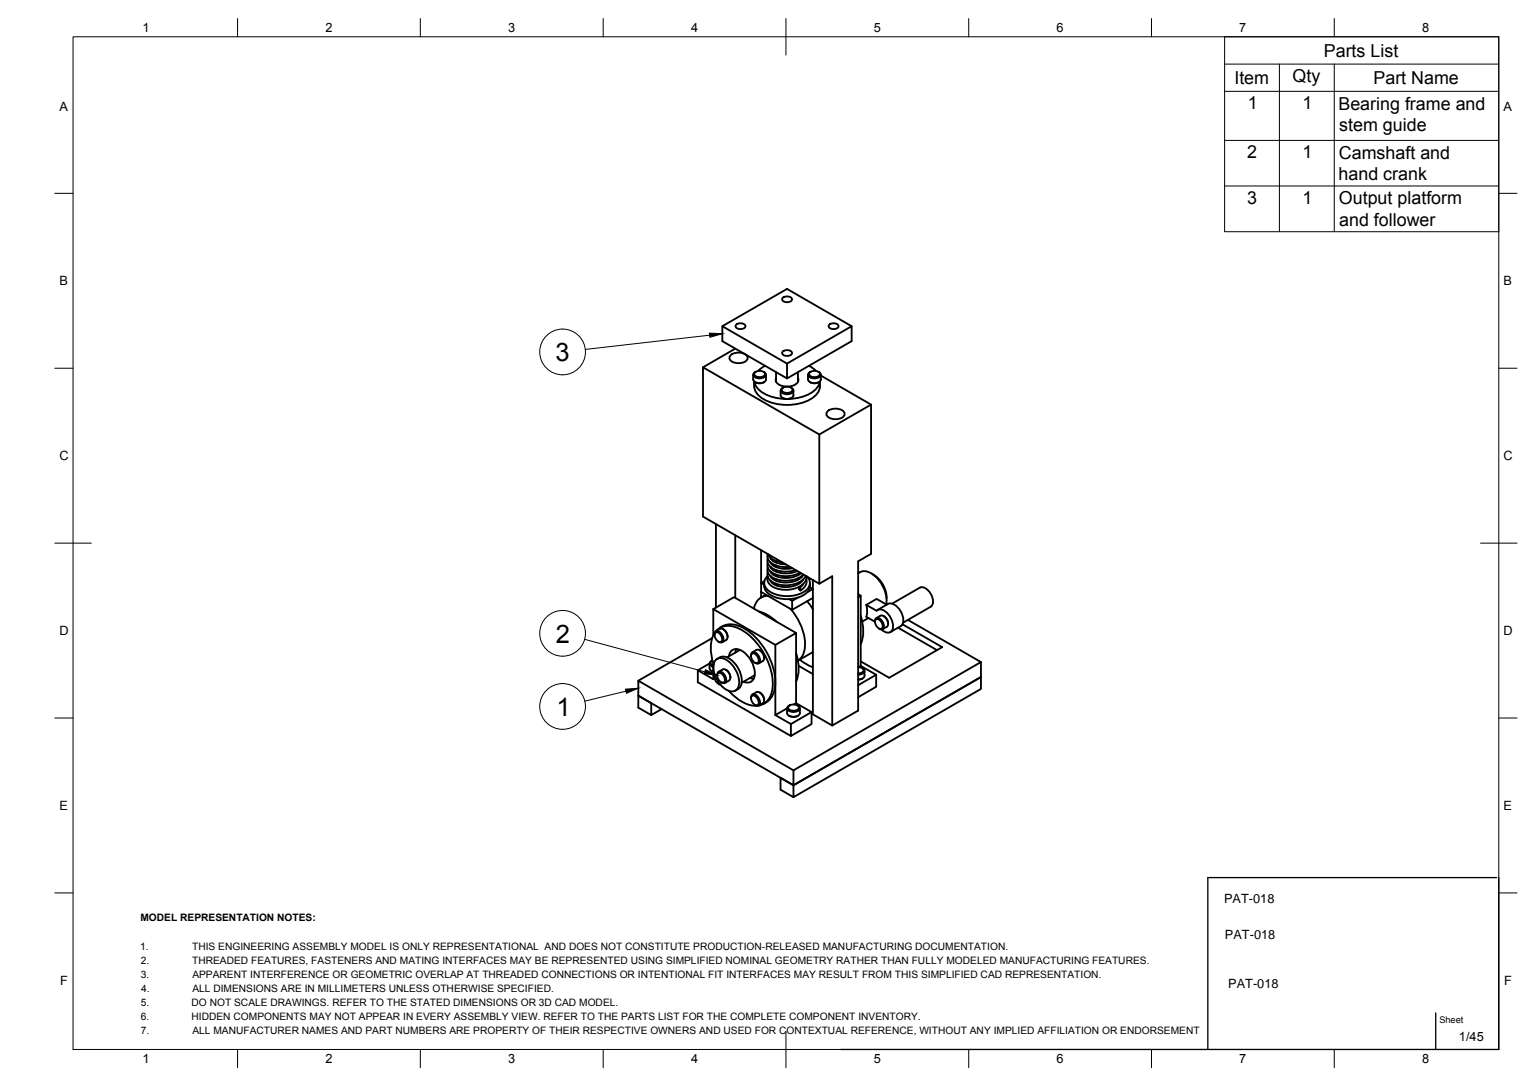
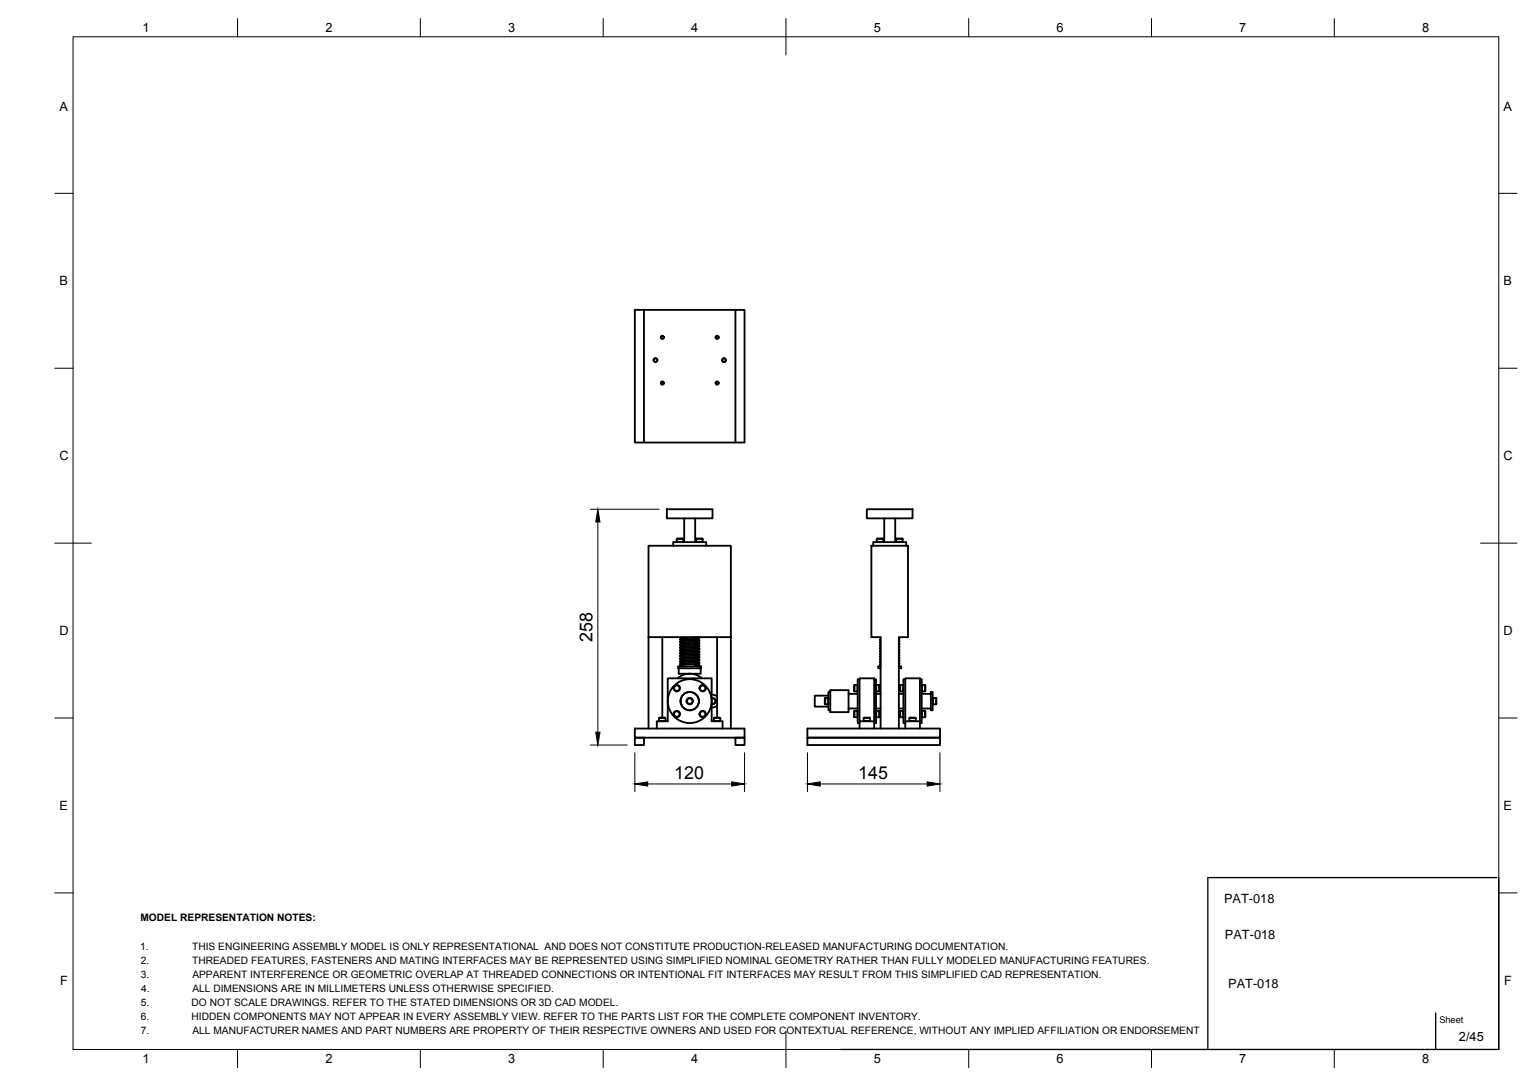
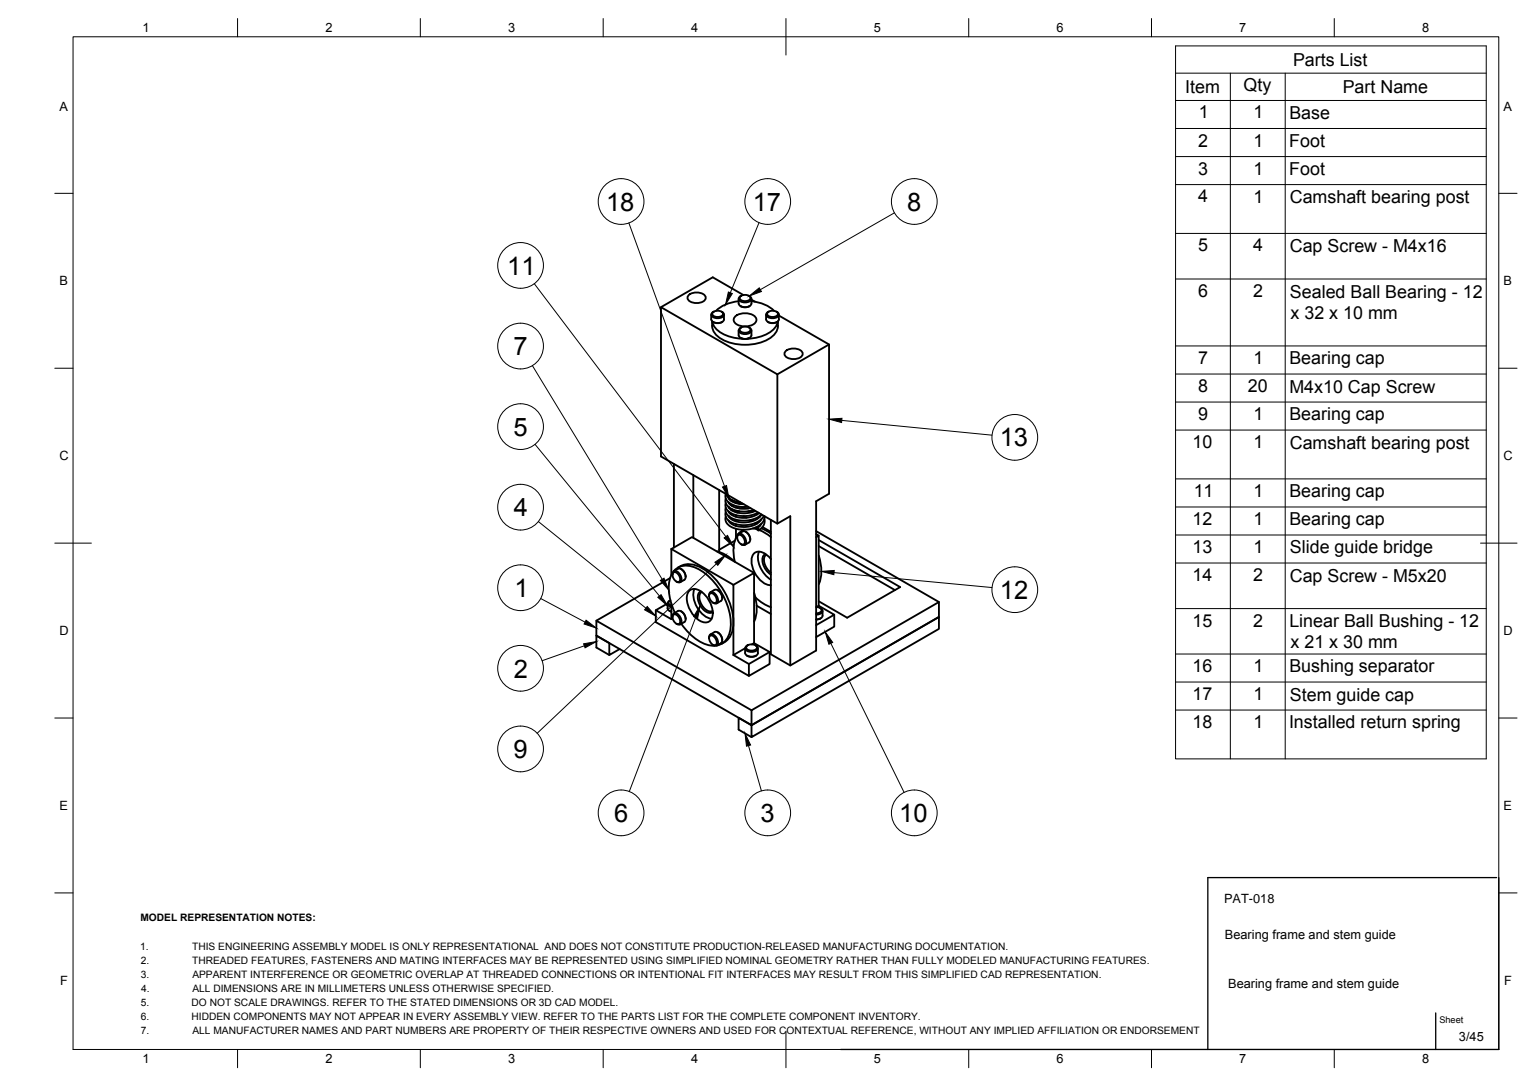
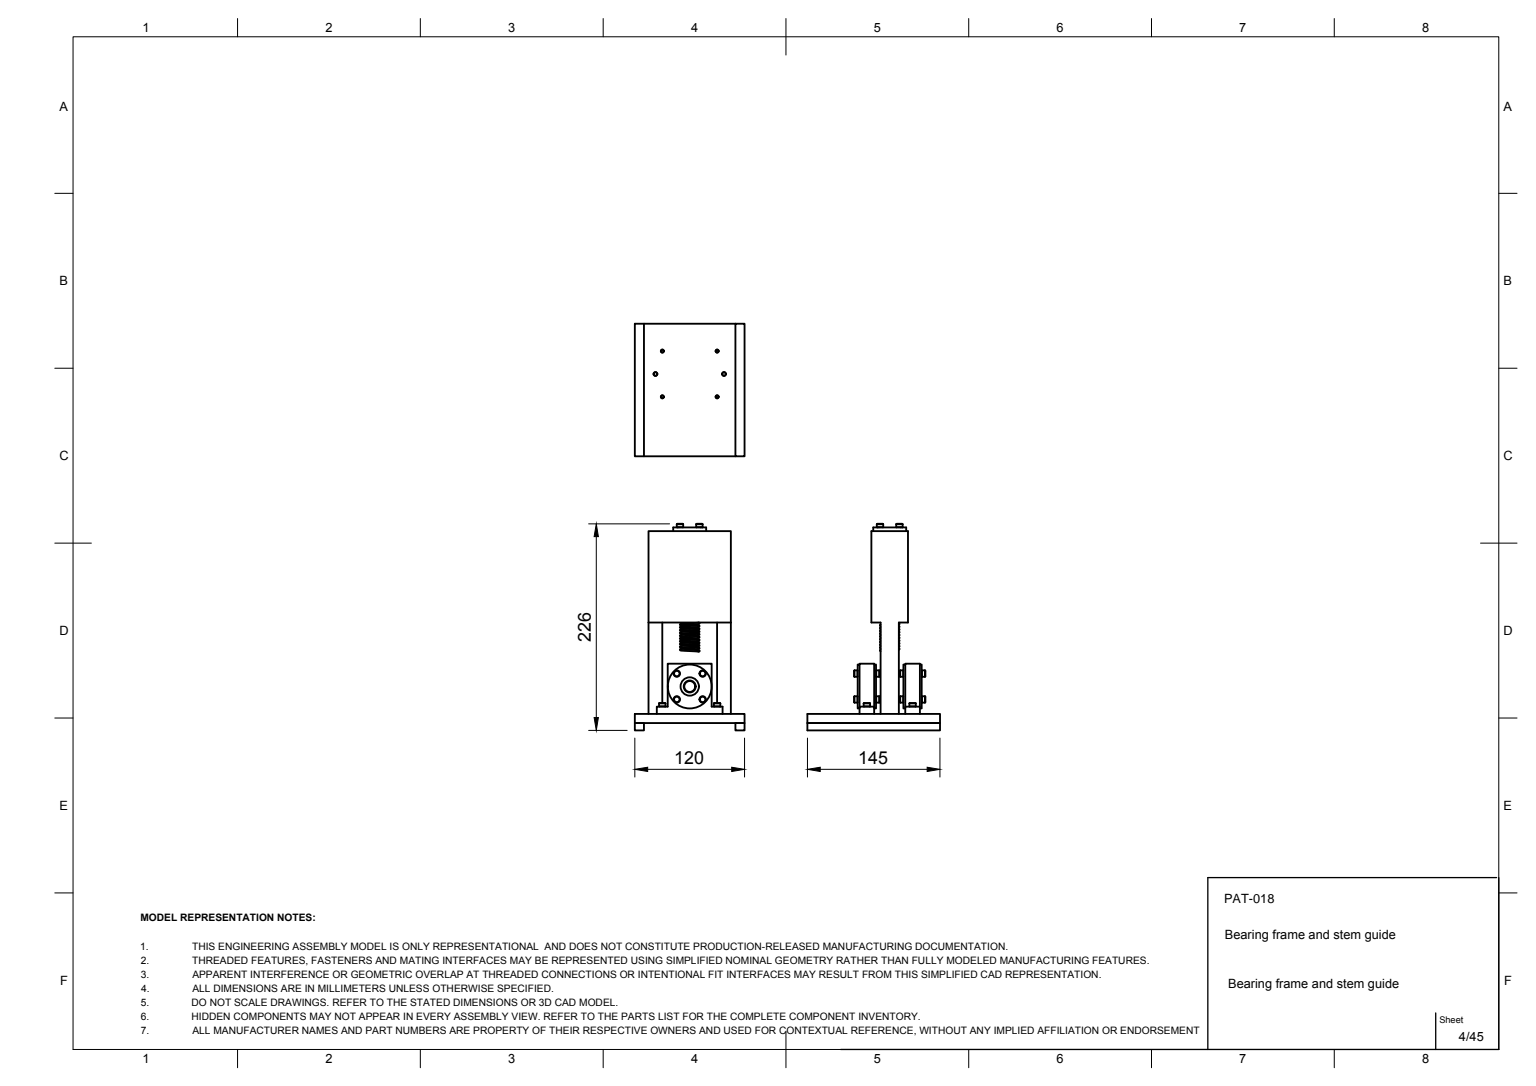
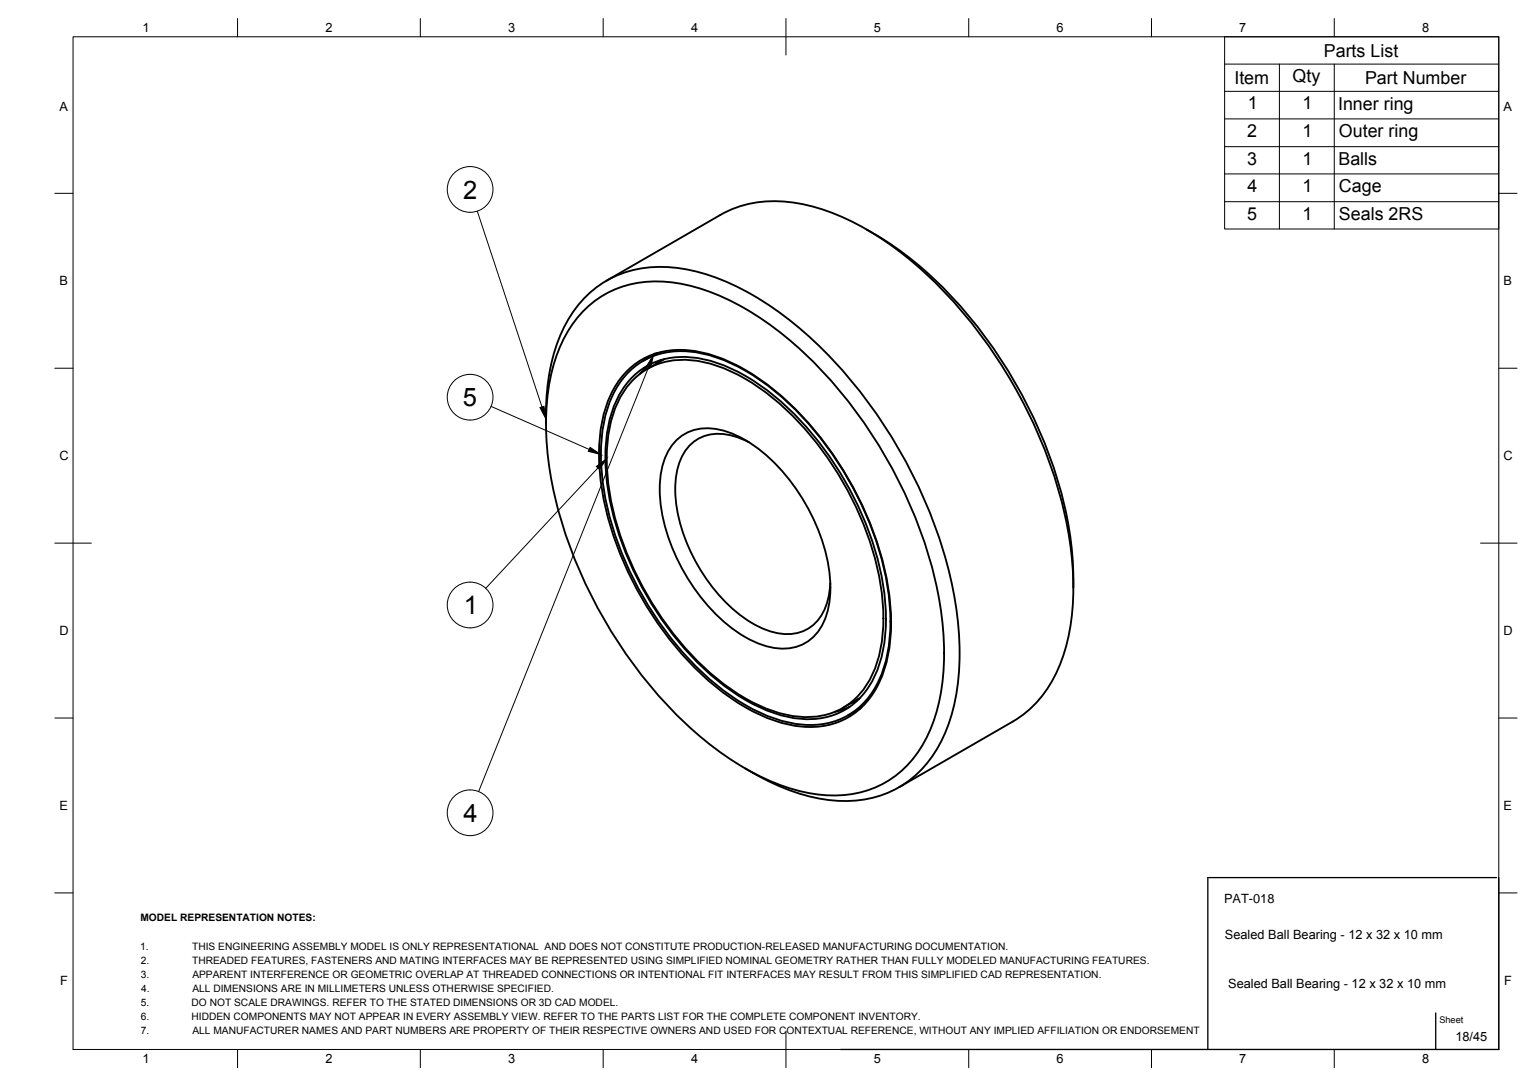
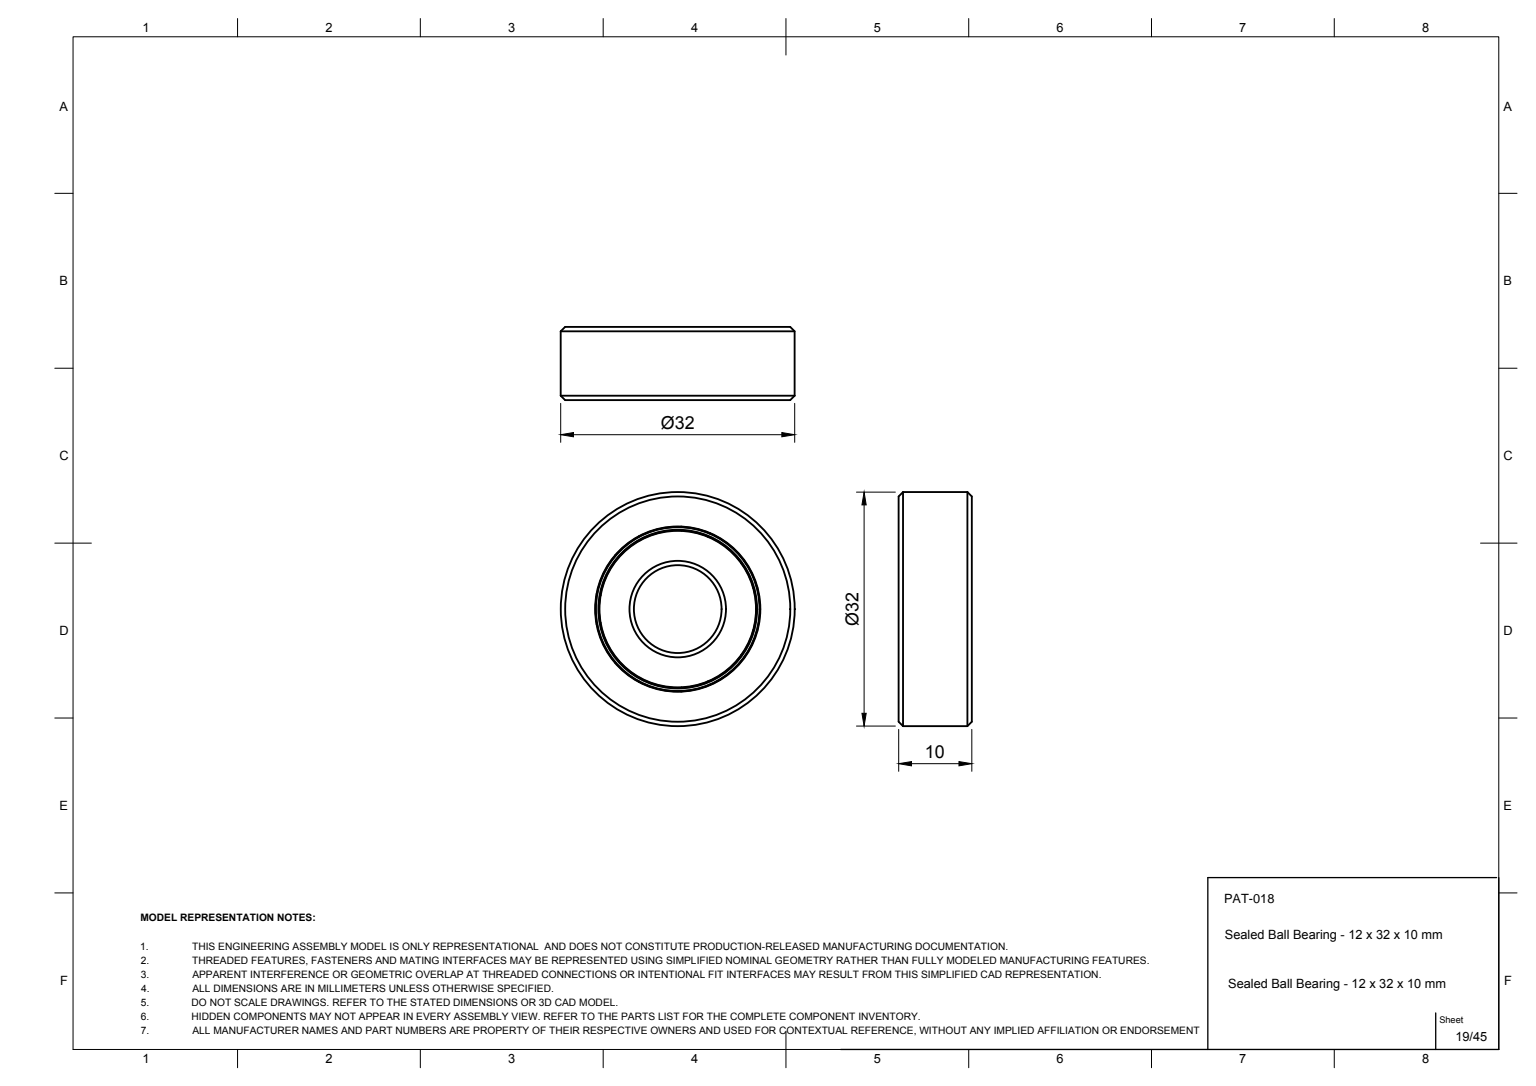
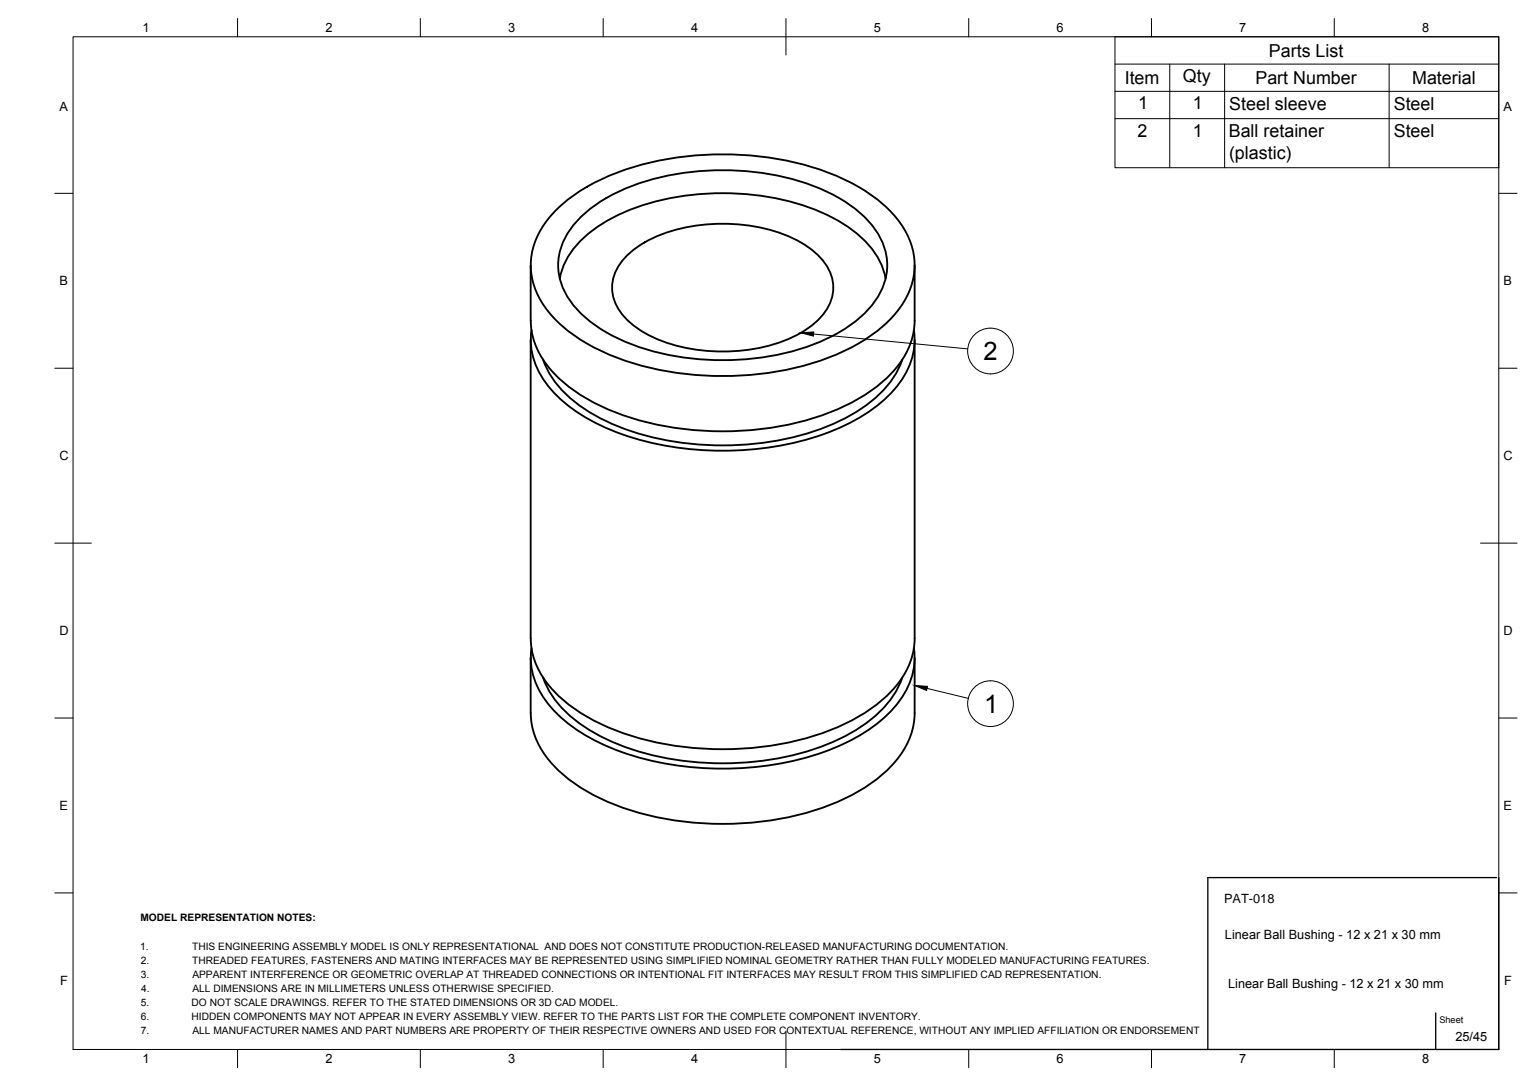
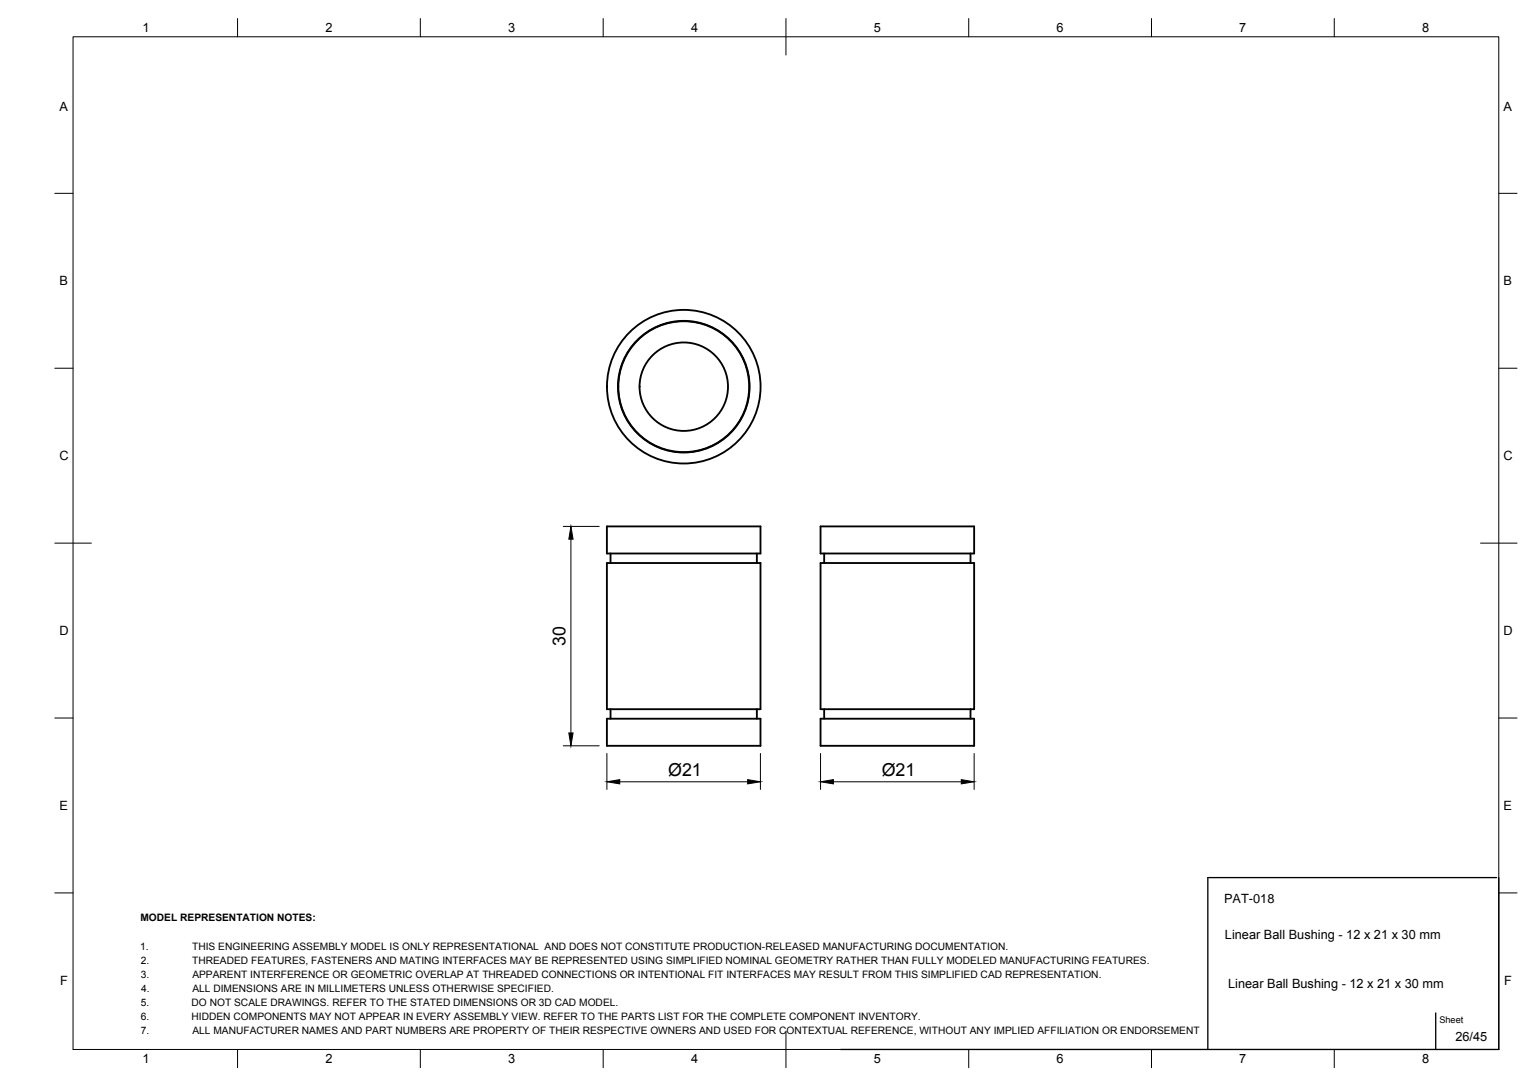
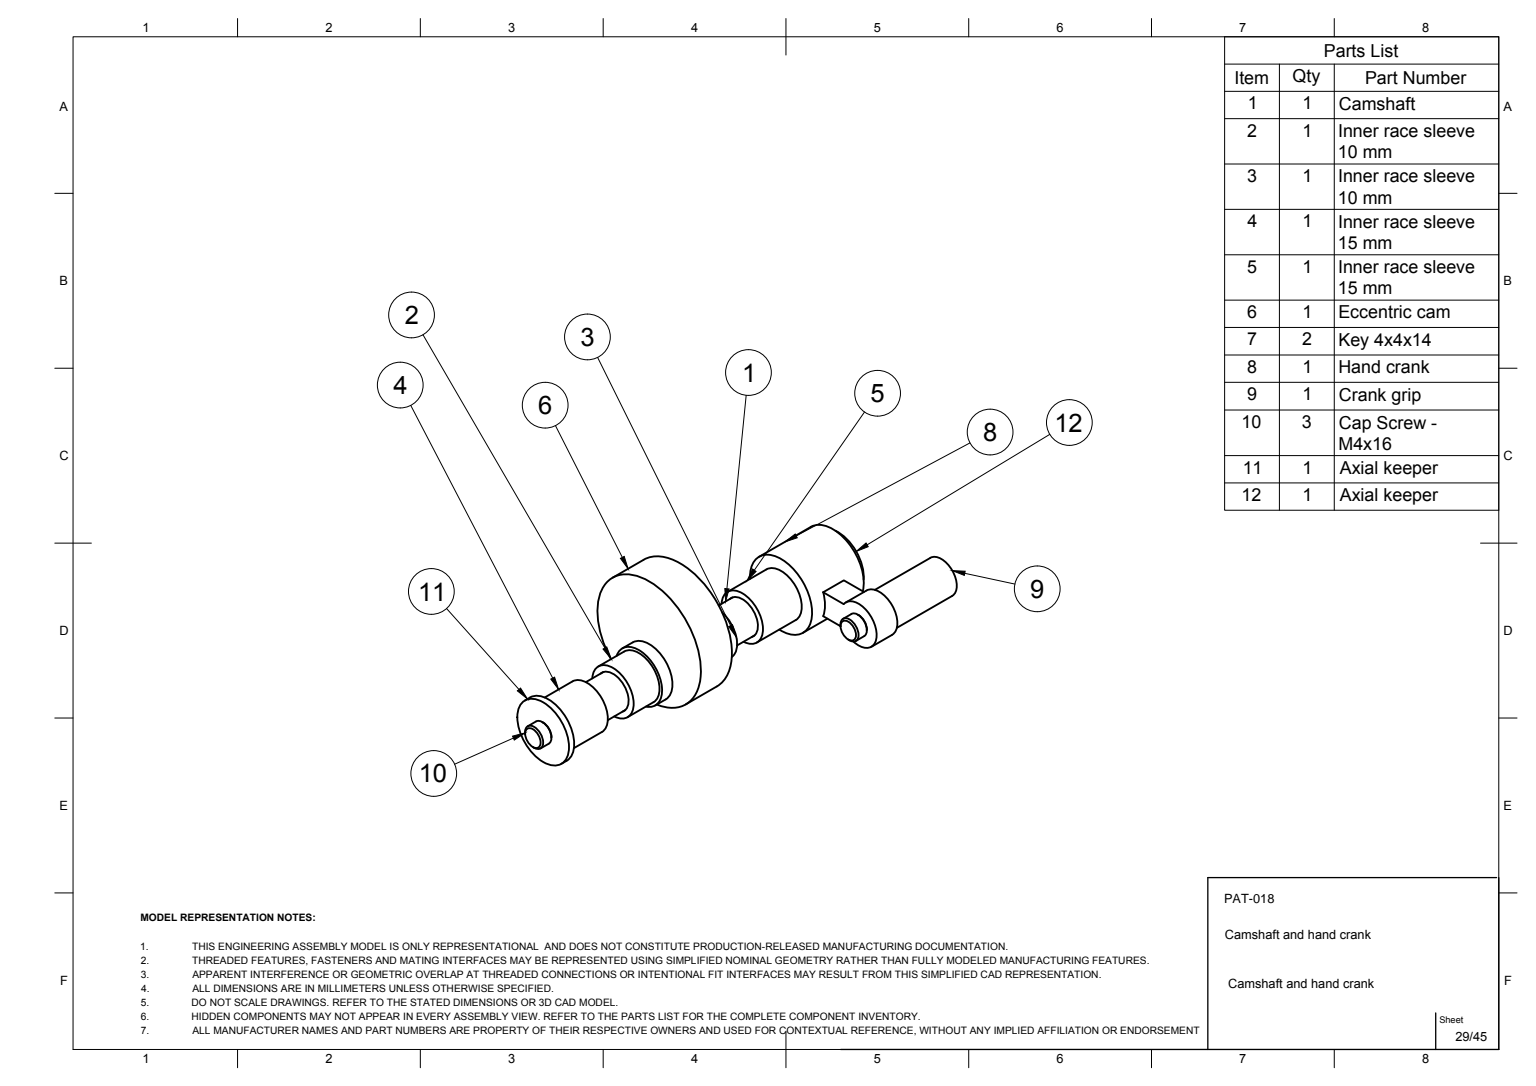
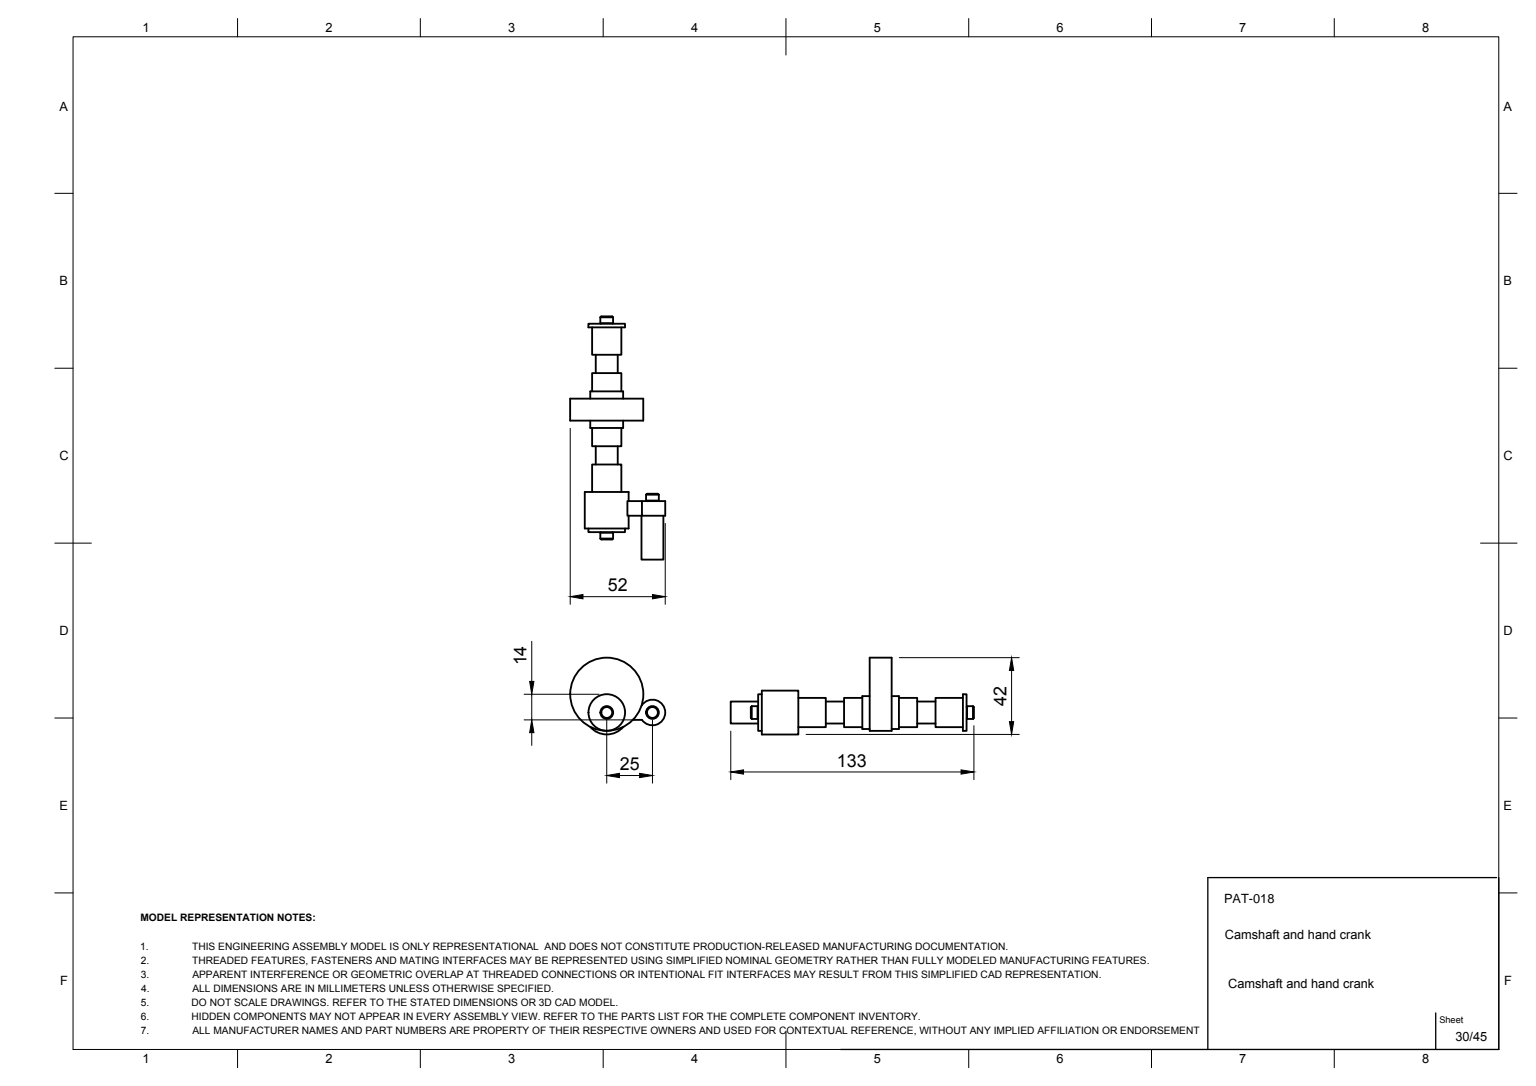
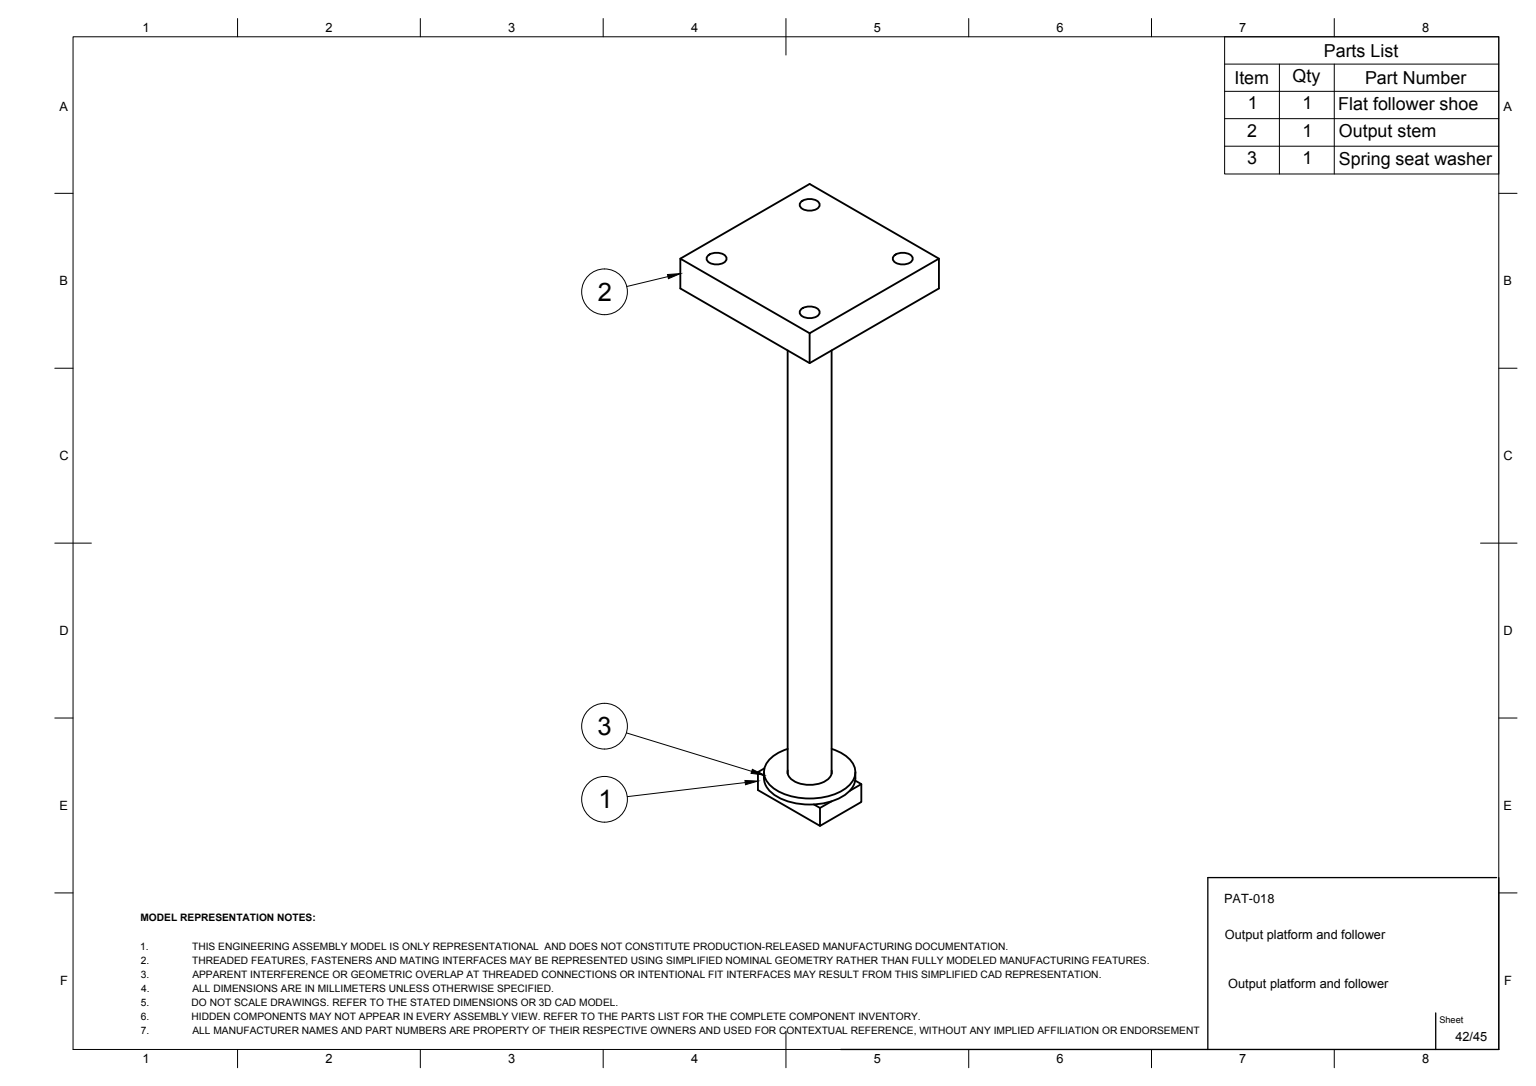
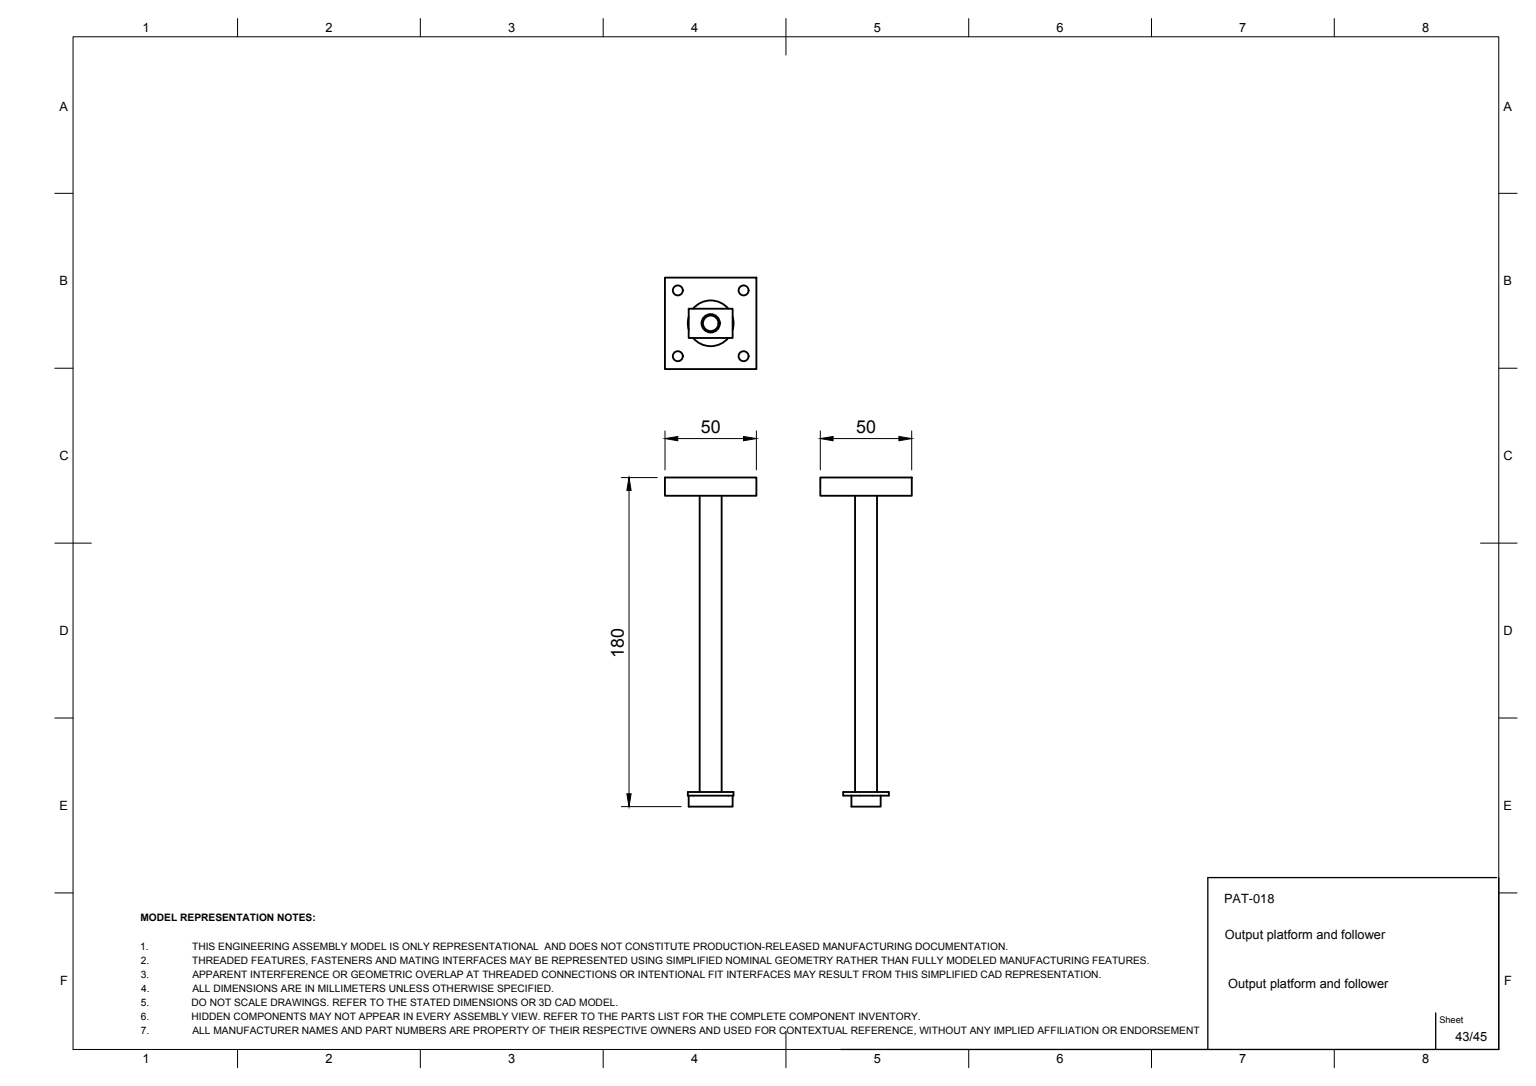
ISO-10303-21;
HEADER;
/* Generated by software containing ST-Developer
 * from STEP Tools, Inc. (www.steptools.com) 
 */

FILE_DESCRIPTION(
/* description */ ('Cam-driven reciprocating slide'),
/* implementation_level */ '2;1');

FILE_NAME(
/* name */ 'PAT-018',
/* time_stamp */ '2026-10-28T03:25:20-07:00',
/* author */ (''),
/* organization */ (''),
/* preprocessor_version */ 'ST-DEVELOPER v20.2',
/* originating_system */ 'Autodesk Translation Framework v15.17.0.0',
/* authorisation */ '');

FILE_SCHEMA (('AUTOMOTIVE_DESIGN { 1 0 10303 214 3 1 1 }'));
ENDSEC;

DATA;
#10=MECHANICAL_DESIGN_GEOMETRIC_PRESENTATION_REPRESENTATION('',(#422,#423,
#424,#425,#426,#427,#428,#429,#430,#431,#432,#433,#434,#435,#436,#437,#438,
#439,#440,#441,#442,#443,#444,#445,#446,#447,#448,#449,#450,#451,#452,#453,
#454,#455,#456,#457,#458,#459,#460,#461,#462,#463,#464,#465),#13277);
#11=ORIENTED_CLOSED_SHELL('',*,#6424,.F.);
#12=ORIENTED_CLOSED_SHELL('',*,#6427,.F.);
#13=ORIENTED_CLOSED_SHELL('',*,#6441,.F.);
#14=BREP_WITH_VOIDS('Body1',#6423,(#11));
#15=BREP_WITH_VOIDS('Body1',#6428,(#12));
#16=BREP_WITH_VOIDS('Body1',#6440,(#13));
#17=ITEM_DEFINED_TRANSFORMATION($,$,#7155,#7277);
#18=ITEM_DEFINED_TRANSFORMATION($,$,#7175,#7278);
#19=ITEM_DEFINED_TRANSFORMATION($,$,#7195,#7279);
#20=ITEM_DEFINED_TRANSFORMATION($,$,#7210,#7280);
#21=ITEM_DEFINED_TRANSFORMATION($,$,#7260,#7281);
#22=ITEM_DEFINED_TRANSFORMATION($,$,#7309,#7358);
#23=ITEM_DEFINED_TRANSFORMATION($,$,#7341,#7359);
#24=ITEM_DEFINED_TRANSFORMATION($,$,#6855,#7558);
#25=ITEM_DEFINED_TRANSFORMATION($,$,#6885,#7559);
#26=ITEM_DEFINED_TRANSFORMATION($,$,#6892,#7560);
#27=ITEM_DEFINED_TRANSFORMATION($,$,#6899,#7561);
#28=ITEM_DEFINED_TRANSFORMATION($,$,#6931,#7562);
#29=ITEM_DEFINED_TRANSFORMATION($,$,#6956,#7563);
#30=ITEM_DEFINED_TRANSFORMATION($,$,#6981,#7564);
#31=ITEM_DEFINED_TRANSFORMATION($,$,#7013,#7565);
#32=ITEM_DEFINED_TRANSFORMATION($,$,#7038,#7566);
#33=ITEM_DEFINED_TRANSFORMATION($,$,#7063,#7567);
#34=ITEM_DEFINED_TRANSFORMATION($,$,#7115,#7568);
#35=ITEM_DEFINED_TRANSFORMATION($,$,#7124,#7569);
#36=ITEM_DEFINED_TRANSFORMATION($,$,#7149,#7570);
#37=ITEM_DEFINED_TRANSFORMATION($,$,#7532,#7571);
#38=ITEM_DEFINED_TRANSFORMATION($,$,#7532,#7572);
#39=ITEM_DEFINED_TRANSFORMATION($,$,#7154,#7573);
#40=ITEM_DEFINED_TRANSFORMATION($,$,#7360,#7574);
#41=ITEM_DEFINED_TRANSFORMATION($,$,#7360,#7575);
#42=ITEM_DEFINED_TRANSFORMATION($,$,#7360,#7576);
#43=ITEM_DEFINED_TRANSFORMATION($,$,#7360,#7577);
#44=ITEM_DEFINED_TRANSFORMATION($,$,#7360,#7578);
#45=ITEM_DEFINED_TRANSFORMATION($,$,#7360,#7579);
#46=ITEM_DEFINED_TRANSFORMATION($,$,#7360,#7580);
#47=ITEM_DEFINED_TRANSFORMATION($,$,#7360,#7581);
#48=ITEM_DEFINED_TRANSFORMATION($,$,#7532,#7582);
#49=ITEM_DEFINED_TRANSFORMATION($,$,#7532,#7583);
#50=ITEM_DEFINED_TRANSFORMATION($,$,#7154,#7584);
#51=ITEM_DEFINED_TRANSFORMATION($,$,#7360,#7585);
#52=ITEM_DEFINED_TRANSFORMATION($,$,#7360,#7586);
#53=ITEM_DEFINED_TRANSFORMATION($,$,#7360,#7587);
#54=ITEM_DEFINED_TRANSFORMATION($,$,#7360,#7588);
#55=ITEM_DEFINED_TRANSFORMATION($,$,#7360,#7589);
#56=ITEM_DEFINED_TRANSFORMATION($,$,#7360,#7590);
#57=ITEM_DEFINED_TRANSFORMATION($,$,#7360,#7591);
#58=ITEM_DEFINED_TRANSFORMATION($,$,#7360,#7592);
#59=ITEM_DEFINED_TRANSFORMATION($,$,#7282,#7593);
#60=ITEM_DEFINED_TRANSFORMATION($,$,#7282,#7594);
#61=ITEM_DEFINED_TRANSFORMATION($,$,#7308,#7595);
#62=ITEM_DEFINED_TRANSFORMATION($,$,#7308,#7596);
#63=ITEM_DEFINED_TRANSFORMATION($,$,#7360,#7597);
#64=ITEM_DEFINED_TRANSFORMATION($,$,#7360,#7598);
#65=ITEM_DEFINED_TRANSFORMATION($,$,#7360,#7599);
#66=ITEM_DEFINED_TRANSFORMATION($,$,#7360,#7600);
#67=ITEM_DEFINED_TRANSFORMATION($,$,#7385,#7601);
#68=ITEM_DEFINED_TRANSFORMATION($,$,#7413,#7602);
#69=ITEM_DEFINED_TRANSFORMATION($,$,#7422,#7603);
#70=ITEM_DEFINED_TRANSFORMATION($,$,#7431,#7604);
#71=ITEM_DEFINED_TRANSFORMATION($,$,#7440,#7605);
#72=ITEM_DEFINED_TRANSFORMATION($,$,#7449,#7606);
#73=ITEM_DEFINED_TRANSFORMATION($,$,#7469,#7607);
#74=ITEM_DEFINED_TRANSFORMATION($,$,#7493,#7608);
#75=ITEM_DEFINED_TRANSFORMATION($,$,#7503,#7609);
#76=ITEM_DEFINED_TRANSFORMATION($,$,#7512,#7610);
#77=ITEM_DEFINED_TRANSFORMATION($,$,#7521,#7611);
#78=ITEM_DEFINED_TRANSFORMATION($,$,#7521,#7612);
#79=ITEM_DEFINED_TRANSFORMATION($,$,#7532,#7613);
#80=ITEM_DEFINED_TRANSFORMATION($,$,#7532,#7614);
#81=ITEM_DEFINED_TRANSFORMATION($,$,#7532,#7615);
#82=ITEM_DEFINED_TRANSFORMATION($,$,#7617,#7663);
#83=ITEM_DEFINED_TRANSFORMATION($,$,#7627,#7664);
#84=ITEM_DEFINED_TRANSFORMATION($,$,#7654,#7665);
#85=ITEM_DEFINED_TRANSFORMATION($,$,#6854,#7666);
#86=ITEM_DEFINED_TRANSFORMATION($,$,#7384,#7667);
#87=ITEM_DEFINED_TRANSFORMATION($,$,#7616,#7668);
#88=(
REPRESENTATION_RELATIONSHIP($,$,#13455,#13454)
REPRESENTATION_RELATIONSHIP_WITH_TRANSFORMATION(#17)
SHAPE_REPRESENTATION_RELATIONSHIP()
);
#89=(
REPRESENTATION_RELATIONSHIP($,$,#13456,#13454)
REPRESENTATION_RELATIONSHIP_WITH_TRANSFORMATION(#18)
SHAPE_REPRESENTATION_RELATIONSHIP()
);
#90=(
REPRESENTATION_RELATIONSHIP($,$,#13457,#13454)
REPRESENTATION_RELATIONSHIP_WITH_TRANSFORMATION(#19)
SHAPE_REPRESENTATION_RELATIONSHIP()
);
#91=(
REPRESENTATION_RELATIONSHIP($,$,#13458,#13454)
REPRESENTATION_RELATIONSHIP_WITH_TRANSFORMATION(#20)
SHAPE_REPRESENTATION_RELATIONSHIP()
);
#92=(
REPRESENTATION_RELATIONSHIP($,$,#13459,#13454)
REPRESENTATION_RELATIONSHIP_WITH_TRANSFORMATION(#21)
SHAPE_REPRESENTATION_RELATIONSHIP()
);
#93=(
REPRESENTATION_RELATIONSHIP($,$,#13462,#13461)
REPRESENTATION_RELATIONSHIP_WITH_TRANSFORMATION(#22)
SHAPE_REPRESENTATION_RELATIONSHIP()
);
#94=(
REPRESENTATION_RELATIONSHIP($,$,#13463,#13461)
REPRESENTATION_RELATIONSHIP_WITH_TRANSFORMATION(#23)
SHAPE_REPRESENTATION_RELATIONSHIP()
);
#95=(
REPRESENTATION_RELATIONSHIP($,$,#13441,#13440)
REPRESENTATION_RELATIONSHIP_WITH_TRANSFORMATION(#24)
SHAPE_REPRESENTATION_RELATIONSHIP()
);
#96=(
REPRESENTATION_RELATIONSHIP($,$,#13442,#13440)
REPRESENTATION_RELATIONSHIP_WITH_TRANSFORMATION(#25)
SHAPE_REPRESENTATION_RELATIONSHIP()
);
#97=(
REPRESENTATION_RELATIONSHIP($,$,#13443,#13440)
REPRESENTATION_RELATIONSHIP_WITH_TRANSFORMATION(#26)
SHAPE_REPRESENTATION_RELATIONSHIP()
);
#98=(
REPRESENTATION_RELATIONSHIP($,$,#13444,#13440)
REPRESENTATION_RELATIONSHIP_WITH_TRANSFORMATION(#27)
SHAPE_REPRESENTATION_RELATIONSHIP()
);
#99=(
REPRESENTATION_RELATIONSHIP($,$,#13445,#13440)
REPRESENTATION_RELATIONSHIP_WITH_TRANSFORMATION(#28)
SHAPE_REPRESENTATION_RELATIONSHIP()
);
#100=(
REPRESENTATION_RELATIONSHIP($,$,#13446,#13440)
REPRESENTATION_RELATIONSHIP_WITH_TRANSFORMATION(#29)
SHAPE_REPRESENTATION_RELATIONSHIP()
);
#101=(
REPRESENTATION_RELATIONSHIP($,$,#13447,#13440)
REPRESENTATION_RELATIONSHIP_WITH_TRANSFORMATION(#30)
SHAPE_REPRESENTATION_RELATIONSHIP()
);
#102=(
REPRESENTATION_RELATIONSHIP($,$,#13448,#13440)
REPRESENTATION_RELATIONSHIP_WITH_TRANSFORMATION(#31)
SHAPE_REPRESENTATION_RELATIONSHIP()
);
#103=(
REPRESENTATION_RELATIONSHIP($,$,#13449,#13440)
REPRESENTATION_RELATIONSHIP_WITH_TRANSFORMATION(#32)
SHAPE_REPRESENTATION_RELATIONSHIP()
);
#104=(
REPRESENTATION_RELATIONSHIP($,$,#13450,#13440)
REPRESENTATION_RELATIONSHIP_WITH_TRANSFORMATION(#33)
SHAPE_REPRESENTATION_RELATIONSHIP()
);
#105=(
REPRESENTATION_RELATIONSHIP($,$,#13451,#13440)
REPRESENTATION_RELATIONSHIP_WITH_TRANSFORMATION(#34)
SHAPE_REPRESENTATION_RELATIONSHIP()
);
#106=(
REPRESENTATION_RELATIONSHIP($,$,#13452,#13440)
REPRESENTATION_RELATIONSHIP_WITH_TRANSFORMATION(#35)
SHAPE_REPRESENTATION_RELATIONSHIP()
);
#107=(
REPRESENTATION_RELATIONSHIP($,$,#13453,#13440)
REPRESENTATION_RELATIONSHIP_WITH_TRANSFORMATION(#36)
SHAPE_REPRESENTATION_RELATIONSHIP()
);
#108=(
REPRESENTATION_RELATIONSHIP($,$,#13477,#13440)
REPRESENTATION_RELATIONSHIP_WITH_TRANSFORMATION(#37)
SHAPE_REPRESENTATION_RELATIONSHIP()
);
#109=(
REPRESENTATION_RELATIONSHIP($,$,#13477,#13440)
REPRESENTATION_RELATIONSHIP_WITH_TRANSFORMATION(#38)
SHAPE_REPRESENTATION_RELATIONSHIP()
);
#110=(
REPRESENTATION_RELATIONSHIP($,$,#13454,#13440)
REPRESENTATION_RELATIONSHIP_WITH_TRANSFORMATION(#39)
SHAPE_REPRESENTATION_RELATIONSHIP()
);
#111=(
REPRESENTATION_RELATIONSHIP($,$,#13464,#13440)
REPRESENTATION_RELATIONSHIP_WITH_TRANSFORMATION(#40)
SHAPE_REPRESENTATION_RELATIONSHIP()
);
#112=(
REPRESENTATION_RELATIONSHIP($,$,#13464,#13440)
REPRESENTATION_RELATIONSHIP_WITH_TRANSFORMATION(#41)
SHAPE_REPRESENTATION_RELATIONSHIP()
);
#113=(
REPRESENTATION_RELATIONSHIP($,$,#13464,#13440)
REPRESENTATION_RELATIONSHIP_WITH_TRANSFORMATION(#42)
SHAPE_REPRESENTATION_RELATIONSHIP()
);
#114=(
REPRESENTATION_RELATIONSHIP($,$,#13464,#13440)
REPRESENTATION_RELATIONSHIP_WITH_TRANSFORMATION(#43)
SHAPE_REPRESENTATION_RELATIONSHIP()
);
#115=(
REPRESENTATION_RELATIONSHIP($,$,#13464,#13440)
REPRESENTATION_RELATIONSHIP_WITH_TRANSFORMATION(#44)
SHAPE_REPRESENTATION_RELATIONSHIP()
);
#116=(
REPRESENTATION_RELATIONSHIP($,$,#13464,#13440)
REPRESENTATION_RELATIONSHIP_WITH_TRANSFORMATION(#45)
SHAPE_REPRESENTATION_RELATIONSHIP()
);
#117=(
REPRESENTATION_RELATIONSHIP($,$,#13464,#13440)
REPRESENTATION_RELATIONSHIP_WITH_TRANSFORMATION(#46)
SHAPE_REPRESENTATION_RELATIONSHIP()
);
#118=(
REPRESENTATION_RELATIONSHIP($,$,#13464,#13440)
REPRESENTATION_RELATIONSHIP_WITH_TRANSFORMATION(#47)
SHAPE_REPRESENTATION_RELATIONSHIP()
);
#119=(
REPRESENTATION_RELATIONSHIP($,$,#13477,#13440)
REPRESENTATION_RELATIONSHIP_WITH_TRANSFORMATION(#48)
SHAPE_REPRESENTATION_RELATIONSHIP()
);
#120=(
REPRESENTATION_RELATIONSHIP($,$,#13477,#13440)
REPRESENTATION_RELATIONSHIP_WITH_TRANSFORMATION(#49)
SHAPE_REPRESENTATION_RELATIONSHIP()
);
#121=(
REPRESENTATION_RELATIONSHIP($,$,#13454,#13440)
REPRESENTATION_RELATIONSHIP_WITH_TRANSFORMATION(#50)
SHAPE_REPRESENTATION_RELATIONSHIP()
);
#122=(
REPRESENTATION_RELATIONSHIP($,$,#13464,#13440)
REPRESENTATION_RELATIONSHIP_WITH_TRANSFORMATION(#51)
SHAPE_REPRESENTATION_RELATIONSHIP()
);
#123=(
REPRESENTATION_RELATIONSHIP($,$,#13464,#13440)
REPRESENTATION_RELATIONSHIP_WITH_TRANSFORMATION(#52)
SHAPE_REPRESENTATION_RELATIONSHIP()
);
#124=(
REPRESENTATION_RELATIONSHIP($,$,#13464,#13440)
REPRESENTATION_RELATIONSHIP_WITH_TRANSFORMATION(#53)
SHAPE_REPRESENTATION_RELATIONSHIP()
);
#125=(
REPRESENTATION_RELATIONSHIP($,$,#13464,#13440)
REPRESENTATION_RELATIONSHIP_WITH_TRANSFORMATION(#54)
SHAPE_REPRESENTATION_RELATIONSHIP()
);
#126=(
REPRESENTATION_RELATIONSHIP($,$,#13464,#13440)
REPRESENTATION_RELATIONSHIP_WITH_TRANSFORMATION(#55)
SHAPE_REPRESENTATION_RELATIONSHIP()
);
#127=(
REPRESENTATION_RELATIONSHIP($,$,#13464,#13440)
REPRESENTATION_RELATIONSHIP_WITH_TRANSFORMATION(#56)
SHAPE_REPRESENTATION_RELATIONSHIP()
);
#128=(
REPRESENTATION_RELATIONSHIP($,$,#13464,#13440)
REPRESENTATION_RELATIONSHIP_WITH_TRANSFORMATION(#57)
SHAPE_REPRESENTATION_RELATIONSHIP()
);
#129=(
REPRESENTATION_RELATIONSHIP($,$,#13464,#13440)
REPRESENTATION_RELATIONSHIP_WITH_TRANSFORMATION(#58)
SHAPE_REPRESENTATION_RELATIONSHIP()
);
#130=(
REPRESENTATION_RELATIONSHIP($,$,#13460,#13440)
REPRESENTATION_RELATIONSHIP_WITH_TRANSFORMATION(#59)
SHAPE_REPRESENTATION_RELATIONSHIP()
);
#131=(
REPRESENTATION_RELATIONSHIP($,$,#13460,#13440)
REPRESENTATION_RELATIONSHIP_WITH_TRANSFORMATION(#60)
SHAPE_REPRESENTATION_RELATIONSHIP()
);
#132=(
REPRESENTATION_RELATIONSHIP($,$,#13461,#13440)
REPRESENTATION_RELATIONSHIP_WITH_TRANSFORMATION(#61)
SHAPE_REPRESENTATION_RELATIONSHIP()
);
#133=(
REPRESENTATION_RELATIONSHIP($,$,#13461,#13440)
REPRESENTATION_RELATIONSHIP_WITH_TRANSFORMATION(#62)
SHAPE_REPRESENTATION_RELATIONSHIP()
);
#134=(
REPRESENTATION_RELATIONSHIP($,$,#13464,#13440)
REPRESENTATION_RELATIONSHIP_WITH_TRANSFORMATION(#63)
SHAPE_REPRESENTATION_RELATIONSHIP()
);
#135=(
REPRESENTATION_RELATIONSHIP($,$,#13464,#13440)
REPRESENTATION_RELATIONSHIP_WITH_TRANSFORMATION(#64)
SHAPE_REPRESENTATION_RELATIONSHIP()
);
#136=(
REPRESENTATION_RELATIONSHIP($,$,#13464,#13440)
REPRESENTATION_RELATIONSHIP_WITH_TRANSFORMATION(#65)
SHAPE_REPRESENTATION_RELATIONSHIP()
);
#137=(
REPRESENTATION_RELATIONSHIP($,$,#13464,#13440)
REPRESENTATION_RELATIONSHIP_WITH_TRANSFORMATION(#66)
SHAPE_REPRESENTATION_RELATIONSHIP()
);
#138=(
REPRESENTATION_RELATIONSHIP($,$,#13466,#13465)
REPRESENTATION_RELATIONSHIP_WITH_TRANSFORMATION(#67)
SHAPE_REPRESENTATION_RELATIONSHIP()
);
#139=(
REPRESENTATION_RELATIONSHIP($,$,#13467,#13465)
REPRESENTATION_RELATIONSHIP_WITH_TRANSFORMATION(#68)
SHAPE_REPRESENTATION_RELATIONSHIP()
);
#140=(
REPRESENTATION_RELATIONSHIP($,$,#13468,#13465)
REPRESENTATION_RELATIONSHIP_WITH_TRANSFORMATION(#69)
SHAPE_REPRESENTATION_RELATIONSHIP()
);
#141=(
REPRESENTATION_RELATIONSHIP($,$,#13469,#13465)
REPRESENTATION_RELATIONSHIP_WITH_TRANSFORMATION(#70)
SHAPE_REPRESENTATION_RELATIONSHIP()
);
#142=(
REPRESENTATION_RELATIONSHIP($,$,#13470,#13465)
REPRESENTATION_RELATIONSHIP_WITH_TRANSFORMATION(#71)
SHAPE_REPRESENTATION_RELATIONSHIP()
);
#143=(
REPRESENTATION_RELATIONSHIP($,$,#13471,#13465)
REPRESENTATION_RELATIONSHIP_WITH_TRANSFORMATION(#72)
SHAPE_REPRESENTATION_RELATIONSHIP()
);
#144=(
REPRESENTATION_RELATIONSHIP($,$,#13472,#13465)
REPRESENTATION_RELATIONSHIP_WITH_TRANSFORMATION(#73)
SHAPE_REPRESENTATION_RELATIONSHIP()
);
#145=(
REPRESENTATION_RELATIONSHIP($,$,#13473,#13465)
REPRESENTATION_RELATIONSHIP_WITH_TRANSFORMATION(#74)
SHAPE_REPRESENTATION_RELATIONSHIP()
);
#146=(
REPRESENTATION_RELATIONSHIP($,$,#13474,#13465)
REPRESENTATION_RELATIONSHIP_WITH_TRANSFORMATION(#75)
SHAPE_REPRESENTATION_RELATIONSHIP()
);
#147=(
REPRESENTATION_RELATIONSHIP($,$,#13475,#13465)
REPRESENTATION_RELATIONSHIP_WITH_TRANSFORMATION(#76)
SHAPE_REPRESENTATION_RELATIONSHIP()
);
#148=(
REPRESENTATION_RELATIONSHIP($,$,#13476,#13465)
REPRESENTATION_RELATIONSHIP_WITH_TRANSFORMATION(#77)
SHAPE_REPRESENTATION_RELATIONSHIP()
);
#149=(
REPRESENTATION_RELATIONSHIP($,$,#13476,#13465)
REPRESENTATION_RELATIONSHIP_WITH_TRANSFORMATION(#78)
SHAPE_REPRESENTATION_RELATIONSHIP()
);
#150=(
REPRESENTATION_RELATIONSHIP($,$,#13477,#13465)
REPRESENTATION_RELATIONSHIP_WITH_TRANSFORMATION(#79)
SHAPE_REPRESENTATION_RELATIONSHIP()
);
#151=(
REPRESENTATION_RELATIONSHIP($,$,#13477,#13465)
REPRESENTATION_RELATIONSHIP_WITH_TRANSFORMATION(#80)
SHAPE_REPRESENTATION_RELATIONSHIP()
);
#152=(
REPRESENTATION_RELATIONSHIP($,$,#13477,#13465)
REPRESENTATION_RELATIONSHIP_WITH_TRANSFORMATION(#81)
SHAPE_REPRESENTATION_RELATIONSHIP()
);
#153=(
REPRESENTATION_RELATIONSHIP($,$,#13479,#13478)
REPRESENTATION_RELATIONSHIP_WITH_TRANSFORMATION(#82)
SHAPE_REPRESENTATION_RELATIONSHIP()
);
#154=(
REPRESENTATION_RELATIONSHIP($,$,#13480,#13478)
REPRESENTATION_RELATIONSHIP_WITH_TRANSFORMATION(#83)
SHAPE_REPRESENTATION_RELATIONSHIP()
);
#155=(
REPRESENTATION_RELATIONSHIP($,$,#13481,#13478)
REPRESENTATION_RELATIONSHIP_WITH_TRANSFORMATION(#84)
SHAPE_REPRESENTATION_RELATIONSHIP()
);
#156=(
REPRESENTATION_RELATIONSHIP($,$,#13440,#13439)
REPRESENTATION_RELATIONSHIP_WITH_TRANSFORMATION(#85)
SHAPE_REPRESENTATION_RELATIONSHIP()
);
#157=(
REPRESENTATION_RELATIONSHIP($,$,#13465,#13439)
REPRESENTATION_RELATIONSHIP_WITH_TRANSFORMATION(#86)
SHAPE_REPRESENTATION_RELATIONSHIP()
);
#158=(
REPRESENTATION_RELATIONSHIP($,$,#13478,#13439)
REPRESENTATION_RELATIONSHIP_WITH_TRANSFORMATION(#87)
SHAPE_REPRESENTATION_RELATIONSHIP()
);
#159=CONTEXT_DEPENDENT_SHAPE_REPRESENTATION(#88,#13346);
#160=CONTEXT_DEPENDENT_SHAPE_REPRESENTATION(#89,#13347);
#161=CONTEXT_DEPENDENT_SHAPE_REPRESENTATION(#90,#13348);
#162=CONTEXT_DEPENDENT_SHAPE_REPRESENTATION(#91,#13349);
#163=CONTEXT_DEPENDENT_SHAPE_REPRESENTATION(#92,#13350);
#164=CONTEXT_DEPENDENT_SHAPE_REPRESENTATION(#93,#13355);
#165=CONTEXT_DEPENDENT_SHAPE_REPRESENTATION(#94,#13356);
#166=CONTEXT_DEPENDENT_SHAPE_REPRESENTATION(#95,#13371);
#167=CONTEXT_DEPENDENT_SHAPE_REPRESENTATION(#96,#13372);
#168=CONTEXT_DEPENDENT_SHAPE_REPRESENTATION(#97,#13373);
#169=CONTEXT_DEPENDENT_SHAPE_REPRESENTATION(#98,#13374);
#170=CONTEXT_DEPENDENT_SHAPE_REPRESENTATION(#99,#13375);
#171=CONTEXT_DEPENDENT_SHAPE_REPRESENTATION(#100,#13376);
#172=CONTEXT_DEPENDENT_SHAPE_REPRESENTATION(#101,#13377);
#173=CONTEXT_DEPENDENT_SHAPE_REPRESENTATION(#102,#13378);
#174=CONTEXT_DEPENDENT_SHAPE_REPRESENTATION(#103,#13379);
#175=CONTEXT_DEPENDENT_SHAPE_REPRESENTATION(#104,#13380);
#176=CONTEXT_DEPENDENT_SHAPE_REPRESENTATION(#105,#13381);
#177=CONTEXT_DEPENDENT_SHAPE_REPRESENTATION(#106,#13382);
#178=CONTEXT_DEPENDENT_SHAPE_REPRESENTATION(#107,#13383);
#179=CONTEXT_DEPENDENT_SHAPE_REPRESENTATION(#108,#13384);
#180=CONTEXT_DEPENDENT_SHAPE_REPRESENTATION(#109,#13385);
#181=CONTEXT_DEPENDENT_SHAPE_REPRESENTATION(#110,#13386);
#182=CONTEXT_DEPENDENT_SHAPE_REPRESENTATION(#111,#13387);
#183=CONTEXT_DEPENDENT_SHAPE_REPRESENTATION(#112,#13388);
#184=CONTEXT_DEPENDENT_SHAPE_REPRESENTATION(#113,#13389);
#185=CONTEXT_DEPENDENT_SHAPE_REPRESENTATION(#114,#13390);
#186=CONTEXT_DEPENDENT_SHAPE_REPRESENTATION(#115,#13391);
#187=CONTEXT_DEPENDENT_SHAPE_REPRESENTATION(#116,#13392);
#188=CONTEXT_DEPENDENT_SHAPE_REPRESENTATION(#117,#13393);
#189=CONTEXT_DEPENDENT_SHAPE_REPRESENTATION(#118,#13394);
#190=CONTEXT_DEPENDENT_SHAPE_REPRESENTATION(#119,#13395);
#191=CONTEXT_DEPENDENT_SHAPE_REPRESENTATION(#120,#13396);
#192=CONTEXT_DEPENDENT_SHAPE_REPRESENTATION(#121,#13397);
#193=CONTEXT_DEPENDENT_SHAPE_REPRESENTATION(#122,#13398);
#194=CONTEXT_DEPENDENT_SHAPE_REPRESENTATION(#123,#13399);
#195=CONTEXT_DEPENDENT_SHAPE_REPRESENTATION(#124,#13400);
#196=CONTEXT_DEPENDENT_SHAPE_REPRESENTATION(#125,#13401);
#197=CONTEXT_DEPENDENT_SHAPE_REPRESENTATION(#126,#13402);
#198=CONTEXT_DEPENDENT_SHAPE_REPRESENTATION(#127,#13403);
#199=CONTEXT_DEPENDENT_SHAPE_REPRESENTATION(#128,#13404);
#200=CONTEXT_DEPENDENT_SHAPE_REPRESENTATION(#129,#13405);
#201=CONTEXT_DEPENDENT_SHAPE_REPRESENTATION(#130,#13406);
#202=CONTEXT_DEPENDENT_SHAPE_REPRESENTATION(#131,#13407);
#203=CONTEXT_DEPENDENT_SHAPE_REPRESENTATION(#132,#13408);
#204=CONTEXT_DEPENDENT_SHAPE_REPRESENTATION(#133,#13409);
#205=CONTEXT_DEPENDENT_SHAPE_REPRESENTATION(#134,#13410);
#206=CONTEXT_DEPENDENT_SHAPE_REPRESENTATION(#135,#13411);
#207=CONTEXT_DEPENDENT_SHAPE_REPRESENTATION(#136,#13412);
#208=CONTEXT_DEPENDENT_SHAPE_REPRESENTATION(#137,#13413);
#209=CONTEXT_DEPENDENT_SHAPE_REPRESENTATION(#138,#13414);
#210=CONTEXT_DEPENDENT_SHAPE_REPRESENTATION(#139,#13415);
#211=CONTEXT_DEPENDENT_SHAPE_REPRESENTATION(#140,#13416);
#212=CONTEXT_DEPENDENT_SHAPE_REPRESENTATION(#141,#13417);
#213=CONTEXT_DEPENDENT_SHAPE_REPRESENTATION(#142,#13418);
#214=CONTEXT_DEPENDENT_SHAPE_REPRESENTATION(#143,#13419);
#215=CONTEXT_DEPENDENT_SHAPE_REPRESENTATION(#144,#13420);
#216=CONTEXT_DEPENDENT_SHAPE_REPRESENTATION(#145,#13421);
#217=CONTEXT_DEPENDENT_SHAPE_REPRESENTATION(#146,#13422);
#218=CONTEXT_DEPENDENT_SHAPE_REPRESENTATION(#147,#13423);
#219=CONTEXT_DEPENDENT_SHAPE_REPRESENTATION(#148,#13424);
#220=CONTEXT_DEPENDENT_SHAPE_REPRESENTATION(#149,#13425);
#221=CONTEXT_DEPENDENT_SHAPE_REPRESENTATION(#150,#13426);
#222=CONTEXT_DEPENDENT_SHAPE_REPRESENTATION(#151,#13427);
#223=CONTEXT_DEPENDENT_SHAPE_REPRESENTATION(#152,#13428);
#224=CONTEXT_DEPENDENT_SHAPE_REPRESENTATION(#153,#13433);
#225=CONTEXT_DEPENDENT_SHAPE_REPRESENTATION(#154,#13434);
#226=CONTEXT_DEPENDENT_SHAPE_REPRESENTATION(#155,#13435);
#227=CONTEXT_DEPENDENT_SHAPE_REPRESENTATION(#156,#13436);
#228=CONTEXT_DEPENDENT_SHAPE_REPRESENTATION(#157,#13437);
#229=CONTEXT_DEPENDENT_SHAPE_REPRESENTATION(#158,#13438);
#230=NEXT_ASSEMBLY_USAGE_OCCURRENCE('Inner ring:1','Inner ring:1',
'Inner ring:1',#13498,#13499,'Inner ring:1');
#231=NEXT_ASSEMBLY_USAGE_OCCURRENCE('Outer ring:1','Outer ring:1',
'Outer ring:1',#13498,#13500,'Outer ring:1');
#232=NEXT_ASSEMBLY_USAGE_OCCURRENCE('Balls:1','Balls:1','Balls:1',#13498,
#13501,'Balls:1');
#233=NEXT_ASSEMBLY_USAGE_OCCURRENCE('Cage:1','Cage:1','Cage:1',#13498,#13502,
'Cage:1');
#234=NEXT_ASSEMBLY_USAGE_OCCURRENCE('Seals 2RS:1','Seals 2RS:1',
'Seals 2RS:1',#13498,#13503,'Seals 2RS:1');
#235=NEXT_ASSEMBLY_USAGE_OCCURRENCE('Steel sleeve:1','Steel sleeve:1',
'Steel sleeve:1',#13505,#13506,'Steel sleeve:1');
#236=NEXT_ASSEMBLY_USAGE_OCCURRENCE('Ball retainer (plastic):1',
'Ball retainer (plastic):1','Ball retainer (plastic):1',#13505,#13507,
'Ball retainer (plastic):1');
#237=NEXT_ASSEMBLY_USAGE_OCCURRENCE('Base:1','Base:1','Base:1',#13484,#13485,
'Base:1');
#238=NEXT_ASSEMBLY_USAGE_OCCURRENCE('Foot:1','Foot:1','Foot:1',#13484,#13486,
'Foot:1');
#239=NEXT_ASSEMBLY_USAGE_OCCURRENCE('Foot (1):1','Foot (1):1',
'Foot (1):1',#13484,#13487,'Foot (1):1');
#240=NEXT_ASSEMBLY_USAGE_OCCURRENCE('Camshaft bearing post:1',
'Camshaft bearing post:1','Camshaft bearing post:1',#13484,#13488,
'Camshaft bearing post:1');
#241=NEXT_ASSEMBLY_USAGE_OCCURRENCE('Bearing cap:1','Bearing cap:1',
'Bearing cap:1',#13484,#13489,'Bearing cap:1');
#242=NEXT_ASSEMBLY_USAGE_OCCURRENCE('Bearing cap (1):1',
'Bearing cap (1):1','Bearing cap (1):1',#13484,#13490,
'Bearing cap (1):1');
#243=NEXT_ASSEMBLY_USAGE_OCCURRENCE('Camshaft bearing post (1):1',
'Camshaft bearing post (1):1','Camshaft bearing post (1):1',#13484,#13491,
'Camshaft bearing post (1):1');
#244=NEXT_ASSEMBLY_USAGE_OCCURRENCE('Bearing cap (2):1',
'Bearing cap (2):1','Bearing cap (2):1',#13484,#13492,
'Bearing cap (2):1');
#245=NEXT_ASSEMBLY_USAGE_OCCURRENCE('Bearing cap (3):1',
'Bearing cap (3):1','Bearing cap (3):1',#13484,#13493,
'Bearing cap (3):1');
#246=NEXT_ASSEMBLY_USAGE_OCCURRENCE('Slide guide bridge:1',
'Slide guide bridge:1','Slide guide bridge:1',#13484,#13494,
'Slide guide bridge:1');
#247=NEXT_ASSEMBLY_USAGE_OCCURRENCE('Bushing separator:1',
'Bushing separator:1','Bushing separator:1',#13484,#13495,
'Bushing separator:1');
#248=NEXT_ASSEMBLY_USAGE_OCCURRENCE('Stem guide cap:1',
'Stem guide cap:1','Stem guide cap:1',#13484,#13496,'Stem guide cap:1');
#249=NEXT_ASSEMBLY_USAGE_OCCURRENCE('Installed return spring:1',
'Installed return spring:1','Installed return spring:1',#13484,#13497,
'Installed return spring:1');
#250=NEXT_ASSEMBLY_USAGE_OCCURRENCE('Cap Screw - M4x16:2',
'Cap Screw - M4x16:2','Cap Screw - M4x16:2',#13484,#13521,
'Cap Screw - M4x16:2');
#251=NEXT_ASSEMBLY_USAGE_OCCURRENCE('Cap Screw - M4x16:3',
'Cap Screw - M4x16:3','Cap Screw - M4x16:3',#13484,#13521,
'Cap Screw - M4x16:3');
#252=NEXT_ASSEMBLY_USAGE_OCCURRENCE(
'Sealed Ball Bearing - 12 x 32 x 10 mm:2',
'Sealed Ball Bearing - 12 x 32 x 10 mm:2',
'Sealed Ball Bearing - 12 x 32 x 10 mm:2',#13484,#13498,
'Sealed Ball Bearing - 12 x 32 x 10 mm:2');
#253=NEXT_ASSEMBLY_USAGE_OCCURRENCE('M4x10 Cap Screw:2',
'M4x10 Cap Screw:2','M4x10 Cap Screw:2',#13484,#13508,
'M4x10 Cap Screw:2');
#254=NEXT_ASSEMBLY_USAGE_OCCURRENCE('M4x10 Cap Screw:3',
'M4x10 Cap Screw:3','M4x10 Cap Screw:3',#13484,#13508,
'M4x10 Cap Screw:3');
#255=NEXT_ASSEMBLY_USAGE_OCCURRENCE('M4x10 Cap Screw:4',
'M4x10 Cap Screw:4','M4x10 Cap Screw:4',#13484,#13508,
'M4x10 Cap Screw:4');
#256=NEXT_ASSEMBLY_USAGE_OCCURRENCE('M4x10 Cap Screw:5',
'M4x10 Cap Screw:5','M4x10 Cap Screw:5',#13484,#13508,
'M4x10 Cap Screw:5');
#257=NEXT_ASSEMBLY_USAGE_OCCURRENCE('M4x10 Cap Screw:6',
'M4x10 Cap Screw:6','M4x10 Cap Screw:6',#13484,#13508,
'M4x10 Cap Screw:6');
#258=NEXT_ASSEMBLY_USAGE_OCCURRENCE('M4x10 Cap Screw:7',
'M4x10 Cap Screw:7','M4x10 Cap Screw:7',#13484,#13508,
'M4x10 Cap Screw:7');
#259=NEXT_ASSEMBLY_USAGE_OCCURRENCE('M4x10 Cap Screw:8',
'M4x10 Cap Screw:8','M4x10 Cap Screw:8',#13484,#13508,
'M4x10 Cap Screw:8');
#260=NEXT_ASSEMBLY_USAGE_OCCURRENCE('M4x10 Cap Screw:9',
'M4x10 Cap Screw:9','M4x10 Cap Screw:9',#13484,#13508,
'M4x10 Cap Screw:9');
#261=NEXT_ASSEMBLY_USAGE_OCCURRENCE('Cap Screw - M4x16:4',
'Cap Screw - M4x16:4','Cap Screw - M4x16:4',#13484,#13521,
'Cap Screw - M4x16:4');
#262=NEXT_ASSEMBLY_USAGE_OCCURRENCE('Cap Screw - M4x16:5',
'Cap Screw - M4x16:5','Cap Screw - M4x16:5',#13484,#13521,
'Cap Screw - M4x16:5');
#263=NEXT_ASSEMBLY_USAGE_OCCURRENCE(
'Sealed Ball Bearing - 12 x 32 x 10 mm:3',
'Sealed Ball Bearing - 12 x 32 x 10 mm:3',
'Sealed Ball Bearing - 12 x 32 x 10 mm:3',#13484,#13498,
'Sealed Ball Bearing - 12 x 32 x 10 mm:3');
#264=NEXT_ASSEMBLY_USAGE_OCCURRENCE('M4x10 Cap Screw:10',
'M4x10 Cap Screw:10','M4x10 Cap Screw:10',#13484,#13508,
'M4x10 Cap Screw:10');
#265=NEXT_ASSEMBLY_USAGE_OCCURRENCE('M4x10 Cap Screw:11',
'M4x10 Cap Screw:11','M4x10 Cap Screw:11',#13484,#13508,
'M4x10 Cap Screw:11');
#266=NEXT_ASSEMBLY_USAGE_OCCURRENCE('M4x10 Cap Screw:12',
'M4x10 Cap Screw:12','M4x10 Cap Screw:12',#13484,#13508,
'M4x10 Cap Screw:12');
#267=NEXT_ASSEMBLY_USAGE_OCCURRENCE('M4x10 Cap Screw:13',
'M4x10 Cap Screw:13','M4x10 Cap Screw:13',#13484,#13508,
'M4x10 Cap Screw:13');
#268=NEXT_ASSEMBLY_USAGE_OCCURRENCE('M4x10 Cap Screw:14',
'M4x10 Cap Screw:14','M4x10 Cap Screw:14',#13484,#13508,
'M4x10 Cap Screw:14');
#269=NEXT_ASSEMBLY_USAGE_OCCURRENCE('M4x10 Cap Screw:15',
'M4x10 Cap Screw:15','M4x10 Cap Screw:15',#13484,#13508,
'M4x10 Cap Screw:15');
#270=NEXT_ASSEMBLY_USAGE_OCCURRENCE('M4x10 Cap Screw:16',
'M4x10 Cap Screw:16','M4x10 Cap Screw:16',#13484,#13508,
'M4x10 Cap Screw:16');
#271=NEXT_ASSEMBLY_USAGE_OCCURRENCE('M4x10 Cap Screw:17',
'M4x10 Cap Screw:17','M4x10 Cap Screw:17',#13484,#13508,
'M4x10 Cap Screw:17');
#272=NEXT_ASSEMBLY_USAGE_OCCURRENCE('Cap Screw - M5x20:2',
'Cap Screw - M5x20:2','Cap Screw - M5x20:2',#13484,#13504,
'Cap Screw - M5x20:2');
#273=NEXT_ASSEMBLY_USAGE_OCCURRENCE('Cap Screw - M5x20:3',
'Cap Screw - M5x20:3','Cap Screw - M5x20:3',#13484,#13504,
'Cap Screw - M5x20:3');
#274=NEXT_ASSEMBLY_USAGE_OCCURRENCE(
'Linear Ball Bushing - 12 x 21 x 30 mm:2',
'Linear Ball Bushing - 12 x 21 x 30 mm:2',
'Linear Ball Bushing - 12 x 21 x 30 mm:2',#13484,#13505,
'Linear Ball Bushing - 12 x 21 x 30 mm:2');
#275=NEXT_ASSEMBLY_USAGE_OCCURRENCE(
'Linear Ball Bushing - 12 x 21 x 30 mm:3',
'Linear Ball Bushing - 12 x 21 x 30 mm:3',
'Linear Ball Bushing - 12 x 21 x 30 mm:3',#13484,#13505,
'Linear Ball Bushing - 12 x 21 x 30 mm:3');
#276=NEXT_ASSEMBLY_USAGE_OCCURRENCE('M4x10 Cap Screw:18',
'M4x10 Cap Screw:18','M4x10 Cap Screw:18',#13484,#13508,
'M4x10 Cap Screw:18');
#277=NEXT_ASSEMBLY_USAGE_OCCURRENCE('M4x10 Cap Screw:19',
'M4x10 Cap Screw:19','M4x10 Cap Screw:19',#13484,#13508,
'M4x10 Cap Screw:19');
#278=NEXT_ASSEMBLY_USAGE_OCCURRENCE('M4x10 Cap Screw:20',
'M4x10 Cap Screw:20','M4x10 Cap Screw:20',#13484,#13508,
'M4x10 Cap Screw:20');
#279=NEXT_ASSEMBLY_USAGE_OCCURRENCE('M4x10 Cap Screw:21',
'M4x10 Cap Screw:21','M4x10 Cap Screw:21',#13484,#13508,
'M4x10 Cap Screw:21');
#280=NEXT_ASSEMBLY_USAGE_OCCURRENCE('Camshaft:1','Camshaft:1',
'Camshaft:1',#13509,#13510,'Camshaft:1');
#281=NEXT_ASSEMBLY_USAGE_OCCURRENCE('Inner race sleeve 10 mm:1',
'Inner race sleeve 10 mm:1','Inner race sleeve 10 mm:1',#13509,#13511,
'Inner race sleeve 10 mm:1');
#282=NEXT_ASSEMBLY_USAGE_OCCURRENCE('Inner race sleeve 10 mm (1):1',
'Inner race sleeve 10 mm (1):1','Inner race sleeve 10 mm (1):1',#13509,
#13512,'Inner race sleeve 10 mm (1):1');
#283=NEXT_ASSEMBLY_USAGE_OCCURRENCE('Inner race sleeve 15 mm:1',
'Inner race sleeve 15 mm:1','Inner race sleeve 15 mm:1',#13509,#13513,
'Inner race sleeve 15 mm:1');
#284=NEXT_ASSEMBLY_USAGE_OCCURRENCE('Inner race sleeve 15 mm (1):1',
'Inner race sleeve 15 mm (1):1','Inner race sleeve 15 mm (1):1',#13509,
#13514,'Inner race sleeve 15 mm (1):1');
#285=NEXT_ASSEMBLY_USAGE_OCCURRENCE('Eccentric cam:1','Eccentric cam:1',
'Eccentric cam:1',#13509,#13515,'Eccentric cam:1');
#286=NEXT_ASSEMBLY_USAGE_OCCURRENCE('Hand crank:1','Hand crank:1',
'Hand crank:1',#13509,#13516,'Hand crank:1');
#287=NEXT_ASSEMBLY_USAGE_OCCURRENCE('Crank grip:1','Crank grip:1',
'Crank grip:1',#13509,#13517,'Crank grip:1');
#288=NEXT_ASSEMBLY_USAGE_OCCURRENCE('Axial keeper:1','Axial keeper:1',
'Axial keeper:1',#13509,#13518,'Axial keeper:1');
#289=NEXT_ASSEMBLY_USAGE_OCCURRENCE('Axial keeper (1):1',
'Axial keeper (1):1','Axial keeper (1):1',#13509,#13519,
'Axial keeper (1):1');
#290=NEXT_ASSEMBLY_USAGE_OCCURRENCE('Key 4x4x14:2','Key 4x4x14:2',
'Key 4x4x14:2',#13509,#13520,'Key 4x4x14:2');
#291=NEXT_ASSEMBLY_USAGE_OCCURRENCE('Key 4x4x14:3','Key 4x4x14:3',
'Key 4x4x14:3',#13509,#13520,'Key 4x4x14:3');
#292=NEXT_ASSEMBLY_USAGE_OCCURRENCE('Cap Screw - M4x16:6',
'Cap Screw - M4x16:6','Cap Screw - M4x16:6',#13509,#13521,
'Cap Screw - M4x16:6');
#293=NEXT_ASSEMBLY_USAGE_OCCURRENCE('Cap Screw - M4x16:7',
'Cap Screw - M4x16:7','Cap Screw - M4x16:7',#13509,#13521,
'Cap Screw - M4x16:7');
#294=NEXT_ASSEMBLY_USAGE_OCCURRENCE('Cap Screw - M4x16:8',
'Cap Screw - M4x16:8','Cap Screw - M4x16:8',#13509,#13521,
'Cap Screw - M4x16:8');
#295=NEXT_ASSEMBLY_USAGE_OCCURRENCE('Flat follower shoe:1',
'Flat follower shoe:1','Flat follower shoe:1',#13522,#13523,
'Flat follower shoe:1');
#296=NEXT_ASSEMBLY_USAGE_OCCURRENCE('Output stem:1','Output stem:1',
'Output stem:1',#13522,#13524,'Output stem:1');
#297=NEXT_ASSEMBLY_USAGE_OCCURRENCE('Spring seat washer:1',
'Spring seat washer:1','Spring seat washer:1',#13522,#13525,
'Spring seat washer:1');
#298=NEXT_ASSEMBLY_USAGE_OCCURRENCE('Bearing frame and stem guide:1',
'Bearing frame and stem guide:1','Bearing frame and stem guide:1',#13483,
#13484,'Bearing frame and stem guide:1');
#299=NEXT_ASSEMBLY_USAGE_OCCURRENCE('Camshaft and hand crank:1',
'Camshaft and hand crank:1','Camshaft and hand crank:1',#13483,#13509,
'Camshaft and hand crank:1');
#300=NEXT_ASSEMBLY_USAGE_OCCURRENCE('Output platform and follower:1',
'Output platform and follower:1','Output platform and follower:1',#13483,
#13522,'Output platform and follower:1');
#301=SPHERICAL_SURFACE('',#7196,0.29765);
#302=SPHERICAL_SURFACE('',#7198,0.29765);
#303=SPHERICAL_SURFACE('',#7200,0.29765);
#304=SPHERICAL_SURFACE('',#7202,0.29765);
#305=SPHERICAL_SURFACE('',#7204,0.29765);
#306=SPHERICAL_SURFACE('',#7206,0.29765);
#307=SPHERICAL_SURFACE('',#7208,0.29765);
#308=SPHERICAL_SURFACE('',#7211,0.309556);
#309=SPHERICAL_SURFACE('',#7227,0.309556);
#310=SPHERICAL_SURFACE('',#7232,0.309556);
#311=SPHERICAL_SURFACE('',#7238,0.309556);
#312=SPHERICAL_SURFACE('',#7243,0.309556);
#313=SPHERICAL_SURFACE('',#7248,0.309556);
#314=SPHERICAL_SURFACE('',#7256,0.309556);
#315=CONICAL_SURFACE('',#7167,0.63,0.785398163397448);
#316=CONICAL_SURFACE('',#7174,0.63,0.785398163397448);
#317=CONICAL_SURFACE('',#7187,1.57,0.785398163397449);
#318=CONICAL_SURFACE('',#7191,1.57,0.785398163397449);
#319=CONICAL_SURFACE('',#7285,0.4,0.785398163397448);
#320=CONICAL_SURFACE('',#7289,0.41,0.785398163397448);
#321=CONICAL_SURFACE('',#7293,0.26,0.463647609000806);
#322=CONICAL_SURFACE('',#7297,0.225,0.785398163397448);
#323=CONICAL_SURFACE('',#7373,0.325,0.785398163397448);
#324=CONICAL_SURFACE('',#7377,0.335,0.785398163397448);
#325=CONICAL_SURFACE('',#7381,0.21,0.463647609000806);
#326=CONICAL_SURFACE('',#7535,0.325,0.785398163397448);
#327=CONICAL_SURFACE('',#7539,0.335,0.785398163397448);
#328=CONICAL_SURFACE('',#7543,0.21,0.463647609000806);
#329=CONICAL_SURFACE('',#7547,0.18,0.785398163397448);
#330=TOROIDAL_SURFACE('',#7156,1.1,0.309556);
#331=TOROIDAL_SURFACE('',#7176,1.1,0.309556);
#332=B_SPLINE_CURVE_WITH_KNOTS('',3,(#11701,#11702,#11703,#11704,#11705,
#11706,#11707,#11708,#11709,#11710,#11711,#11712,#11713,#11714,#11715,#11716,
#11717,#11718,#11719,#11720,#11721,#11722,#11723,#11724,#11725,#11726,#11727,
#11728,#11729,#11730,#11731,#11732,#11733,#11734,#11735,#11736,#11737,#11738,
#11739,#11740,#11741,#11742,#11743,#11744,#11745,#11746,#11747,#11748,#11749,
#11750,#11751,#11752,#11753,#11754,#11755,#11756,#11757,#11758,#11759,#11760,
#11761,#11762,#11763,#11764,#11765,#11766,#11767,#11768,#11769,#11770,#11771,
#11772,#11773,#11774,#11775,#11776,#11777,#11778,#11779,#11780,#11781,#11782,
#11783,#11784,#11785,#11786,#11787,#11788,#11789,#11790,#11791,#11792,#11793,
#11794,#11795,#11796,#11797,#11798,#11799,#11800,#11801,#11802,#11803,#11804,
#11805,#11806,#11807,#11808,#11809,#11810,#11811,#11812,#11813,#11814,#11815,
#11816,#11817,#11818,#11819,#11820,#11821,#11822,#11823,#11824),
 .UNSPECIFIED.,.F.,.F.,(4,1,1,1,1,1,1,1,1,1,1,1,1,1,1,1,1,1,1,1,1,1,1,1,
1,1,1,1,1,1,1,1,1,1,1,1,1,1,1,1,1,1,1,1,1,1,1,1,1,1,1,1,1,1,1,1,1,1,1,1,
1,1,1,1,1,1,1,1,1,1,1,1,1,1,1,1,1,1,1,1,1,1,1,1,1,1,1,1,1,1,1,1,1,1,1,1,
1,1,1,1,1,1,1,1,1,1,1,1,1,1,1,1,1,1,1,1,1,1,1,1,1,4),(0.,0.00892857142857143,
0.0178571428571429,0.0267857142857143,0.0357142857142857,0.0446428571428571,
0.0535714285714286,0.0625,0.0714285714285714,0.0803571428571428,0.0892857142857143,
0.0982142857142857,0.107142857142857,0.116071428571429,0.125,0.133928571428571,
0.142857142857143,0.150793650793651,0.154761904761905,0.156746031746032,
0.158730158730159,0.166666666666667,0.174603174603175,0.182539682539683,
0.19047619047619,0.202380952380952,0.214285714285714,0.222222222222222,
0.23015873015873,0.238095238095238,0.244047619047619,0.25,0.261904761904762,
0.273809523809524,0.285714285714286,0.297619047619048,0.30952380952381,
0.321428571428571,0.327380952380952,0.333333333333333,0.341269841269841,
0.349206349206349,0.357142857142857,0.365079365079365,0.373015873015873,
0.380952380952381,0.386904761904762,0.392857142857143,0.404761904761905,
0.416666666666667,0.422619047619048,0.428571428571429,0.4375,0.446428571428571,
0.455357142857143,0.464285714285714,0.468253968253968,0.476190476190476,
0.482142857142857,0.488095238095238,0.494047619047619,0.5,0.504464285714286,
0.508928571428571,0.517857142857143,0.526785714285714,0.535714285714286,
0.540178571428571,0.544642857142857,0.553571428571429,0.5625,0.571428571428571,
0.580357142857143,0.589285714285714,0.598214285714286,0.607142857142857,
0.616071428571429,0.625,0.633928571428571,0.642857142857143,0.650793650793651,
0.658730158730159,0.666666666666667,0.672619047619048,0.678571428571428,
0.69047619047619,0.696428571428571,0.702380952380952,0.714285714285714,
0.726190476190476,0.738095238095238,0.746031746031746,0.753968253968254,
0.761904761904762,0.76984126984127,0.777777777777778,0.785714285714286,
0.790178571428571,0.794642857142857,0.803571428571428,0.8125,0.821428571428571,
0.830357142857143,0.839285714285714,0.848214285714286,0.857142857142857,
0.866071428571429,0.875,0.883928571428571,0.892857142857143,0.901785714285714,
0.910714285714286,0.919642857142857,0.928571428571429,0.9375,0.946428571428571,
0.955357142857143,0.964285714285714,0.973214285714286,0.982142857142857,
0.991071428571429,1.),.UNSPECIFIED.);
#333=B_SPLINE_CURVE_WITH_KNOTS('',3,(#11932,#11933,#11934,#11935,#11936,
#11937,#11938,#11939,#11940,#11941,#11942,#11943,#11944,#11945,#11946,#11947,
#11948,#11949,#11950,#11951,#11952,#11953),.UNSPECIFIED.,.F.,.F.,(4,2,2,
2,2,2,2,2,2,2,4),(0.0591825211272536,0.157966726598481,0.236950089897721,
0.315933453196962,0.391576304923761,0.46721915665056,0.54286200837736,0.618504860104159,
0.697488223403399,0.77647158670264,0.875255792173867),.UNSPECIFIED.);
#334=B_SPLINE_CURVE_WITH_KNOTS('',3,(#11957,#11958,#11959,#11960,#11961,
#11962,#11963,#11964,#11965,#11966,#11967,#11968,#11969,#11970,#11971,#11972,
#11973,#11974,#11975,#11976,#11977,#11978),.UNSPECIFIED.,.F.,.F.,(4,2,2,
2,2,2,2,2,2,2,4),(0.0581119756758434,0.106553146291161,0.213106292582322,
0.30849933801665,0.386091982889075,0.4636846277615,0.541277272633925,0.61886991750635,
0.714262962940678,0.820816109231839,0.869257279847157),.UNSPECIFIED.);
#335=B_SPLINE_CURVE_WITH_KNOTS('',3,(#11984,#11985,#11986,#11987,#11988,
#11989,#11990,#11991,#11992,#11993,#11994,#11995,#11996,#11997,#11998,#11999,
#12000,#12001,#12002,#12003,#12004,#12005),.UNSPECIFIED.,.F.,.F.,(4,2,2,
2,2,2,2,2,2,2,4),(0.0581119756758434,0.106553146291161,0.213106292582322,
0.30849933801665,0.386091982889075,0.4636846277615,0.541277272633925,0.61886991750635,
0.714262962940679,0.820816109231839,0.869257279847157),.UNSPECIFIED.);
#336=B_SPLINE_CURVE_WITH_KNOTS('',3,(#12009,#12010,#12011,#12012,#12013,
#12014,#12015,#12016,#12017,#12018,#12019,#12020,#12021,#12022,#12023,#12024,
#12025,#12026,#12027,#12028,#12029,#12030),.UNSPECIFIED.,.F.,.F.,(4,2,2,
2,2,2,2,2,2,2,4),(0.0581119756758433,0.106553146291161,0.213106292582322,
0.308499338016649,0.386091982889075,0.4636846277615,0.541277272633925,0.61886991750635,
0.714262962940678,0.820816109231839,0.869257279847157),.UNSPECIFIED.);
#337=B_SPLINE_CURVE_WITH_KNOTS('',3,(#12039,#12040,#12041,#12042,#12043,
#12044,#12045,#12046,#12047,#12048,#12049,#12050,#12051,#12052,#12053,#12054,
#12055,#12056,#12057,#12058,#12059,#12060),.UNSPECIFIED.,.F.,.F.,(4,2,2,
2,2,2,2,2,2,2,4),(0.0581119756758433,0.106553146291161,0.213106292582322,
0.30849933801665,0.386091982889075,0.4636846277615,0.541277272633925,0.61886991750635,
0.714262962940678,0.820816109231839,0.869257279847157),.UNSPECIFIED.);
#338=B_SPLINE_CURVE_WITH_KNOTS('',3,(#12064,#12065,#12066,#12067,#12068,
#12069,#12070,#12071,#12072,#12073,#12074,#12075,#12076,#12077,#12078,#12079,
#12080,#12081,#12082,#12083,#12084,#12085),.UNSPECIFIED.,.F.,.F.,(4,2,2,
2,2,2,2,2,2,2,4),(0.0581119756758434,0.106553146291161,0.213106292582322,
0.30849933801665,0.386091982889075,0.4636846277615,0.541277272633925,0.61886991750635,
0.714262962940678,0.820816109231839,0.869257279847157),.UNSPECIFIED.);
#339=B_SPLINE_CURVE_WITH_KNOTS('',3,(#12089,#12090,#12091,#12092,#12093,
#12094,#12095,#12096,#12097,#12098,#12099,#12100,#12101,#12102,#12103,#12104,
#12105,#12106,#12107,#12108,#12109,#12110),.UNSPECIFIED.,.F.,.F.,(4,2,2,
2,2,2,2,2,2,2,4),(0.0581119756758434,0.106553146291161,0.213106292582322,
0.30849933801665,0.386091982889075,0.4636846277615,0.541277272633925,0.61886991750635,
0.714262962940678,0.820816109231839,0.869257279847157),.UNSPECIFIED.);
#340=B_SPLINE_CURVE_WITH_KNOTS('',3,(#12114,#12115,#12116,#12117,#12118,
#12119,#12120,#12121,#12122,#12123,#12124,#12125,#12126,#12127,#12128,#12129,
#12130,#12131,#12132,#12133,#12134,#12135),.UNSPECIFIED.,.F.,.F.,(4,2,2,
2,2,2,2,2,2,2,4),(0.0581119756758433,0.106553146291161,0.213106292582322,
0.30849933801665,0.386091982889075,0.4636846277615,0.541277272633925,0.61886991750635,
0.714262962940678,0.820816109231839,0.869257279847157),.UNSPECIFIED.);
#341=B_SPLINE_CURVE_WITH_KNOTS('',3,(#12143,#12144,#12145,#12146,#12147,
#12148,#12149,#12150,#12151,#12152,#12153,#12154,#12155,#12156,#12157,#12158,
#12159,#12160,#12161,#12162,#12163,#12164),.UNSPECIFIED.,.F.,.F.,(4,2,2,
2,2,2,2,2,2,2,4),(0.0591825211272536,0.157966726598481,0.236950089897721,
0.315933453196962,0.391576304923761,0.467219156650561,0.54286200837736,
0.618504860104159,0.697488223403399,0.77647158670264,0.875255792173867),
 .UNSPECIFIED.);
#342=B_SPLINE_CURVE_WITH_KNOTS('',3,(#12172,#12173,#12174,#12175,#12176,
#12177,#12178,#12179,#12180,#12181,#12182,#12183,#12184,#12185,#12186,#12187,
#12188,#12189,#12190,#12191,#12192,#12193),.UNSPECIFIED.,.F.,.F.,(4,2,2,
2,2,2,2,2,2,2,4),(0.0591825211272536,0.157966726598481,0.236950089897722,
0.315933453196962,0.391576304923761,0.467219156650561,0.54286200837736,
0.618504860104159,0.697488223403399,0.77647158670264,0.875255792173867),
 .UNSPECIFIED.);
#343=B_SPLINE_CURVE_WITH_KNOTS('',3,(#12203,#12204,#12205,#12206,#12207,
#12208,#12209,#12210,#12211,#12212,#12213,#12214,#12215,#12216,#12217,#12218,
#12219,#12220,#12221,#12222,#12223,#12224),.UNSPECIFIED.,.F.,.F.,(4,2,2,
2,2,2,2,2,2,2,4),(0.0591825211272536,0.157966726598481,0.236950089897721,
0.315933453196962,0.391576304923761,0.46721915665056,0.54286200837736,0.618504860104159,
0.697488223403399,0.77647158670264,0.875255792173867),.UNSPECIFIED.);
#344=B_SPLINE_CURVE_WITH_KNOTS('',3,(#12232,#12233,#12234,#12235,#12236,
#12237,#12238,#12239,#12240,#12241,#12242,#12243,#12244,#12245,#12246,#12247,
#12248,#12249,#12250,#12251,#12252,#12253),.UNSPECIFIED.,.F.,.F.,(4,2,2,
2,2,2,2,2,2,2,4),(0.0591825211272536,0.157966726598481,0.236950089897721,
0.315933453196962,0.391576304923761,0.46721915665056,0.542862008377359,
0.618504860104159,0.697488223403399,0.776471586702639,0.875255792173867),
 .UNSPECIFIED.);
#345=B_SPLINE_CURVE_WITH_KNOTS('',3,(#12261,#12262,#12263,#12264,#12265,
#12266,#12267,#12268,#12269,#12270,#12271,#12272,#12273,#12274,#12275,#12276,
#12277,#12278,#12279,#12280,#12281,#12282),.UNSPECIFIED.,.F.,.F.,(4,2,2,
2,2,2,2,2,2,2,4),(0.0591825211272536,0.157966726598481,0.236950089897721,
0.315933453196962,0.391576304923761,0.46721915665056,0.54286200837736,0.618504860104159,
0.697488223403399,0.77647158670264,0.875255792173867),.UNSPECIFIED.);
#346=B_SPLINE_CURVE_WITH_KNOTS('',3,(#12291,#12292,#12293,#12294,#12295,
#12296,#12297,#12298,#12299,#12300,#12301,#12302,#12303,#12304,#12305,#12306,
#12307,#12308,#12309,#12310,#12311,#12312),.UNSPECIFIED.,.F.,.F.,(4,2,2,
2,2,2,2,2,2,2,4),(0.0591825211272536,0.157966726598481,0.236950089897721,
0.315933453196962,0.391576304923761,0.46721915665056,0.542862008377359,
0.618504860104159,0.697488223403399,0.776471586702639,0.875255792173867),
 .UNSPECIFIED.);
#347=B_SPLINE_SURFACE_WITH_KNOTS('',3,3,((#10458,#10459,#10460,#10461,#10462,
#10463,#10464,#10465,#10466,#10467,#10468,#10469,#10470,#10471,#10472,#10473,
#10474,#10475,#10476,#10477,#10478,#10479,#10480,#10481,#10482,#10483,#10484,
#10485,#10486,#10487,#10488,#10489,#10490,#10491,#10492,#10493,#10494,#10495,
#10496,#10497,#10498,#10499,#10500,#10501,#10502,#10503,#10504,#10505,#10506,
#10507,#10508,#10509,#10510,#10511,#10512,#10513,#10514,#10515,#10516,#10517,
#10518,#10519,#10520,#10521,#10522,#10523,#10524,#10525,#10526,#10527,#10528,
#10529,#10530,#10531,#10532,#10533,#10534,#10535,#10536,#10537,#10538,#10539,
#10540,#10541,#10542,#10543,#10544,#10545,#10546,#10547,#10548,#10549,#10550,
#10551,#10552,#10553,#10554,#10555,#10556,#10557,#10558,#10559,#10560,#10561,
#10562,#10563,#10564,#10565,#10566,#10567,#10568,#10569,#10570,#10571,#10572,
#10573,#10574,#10575,#10576,#10577,#10578,#10579,#10580,#10581),(#10582,
#10583,#10584,#10585,#10586,#10587,#10588,#10589,#10590,#10591,#10592,#10593,
#10594,#10595,#10596,#10597,#10598,#10599,#10600,#10601,#10602,#10603,#10604,
#10605,#10606,#10607,#10608,#10609,#10610,#10611,#10612,#10613,#10614,#10615,
#10616,#10617,#10618,#10619,#10620,#10621,#10622,#10623,#10624,#10625,#10626,
#10627,#10628,#10629,#10630,#10631,#10632,#10633,#10634,#10635,#10636,#10637,
#10638,#10639,#10640,#10641,#10642,#10643,#10644,#10645,#10646,#10647,#10648,
#10649,#10650,#10651,#10652,#10653,#10654,#10655,#10656,#10657,#10658,#10659,
#10660,#10661,#10662,#10663,#10664,#10665,#10666,#10667,#10668,#10669,#10670,
#10671,#10672,#10673,#10674,#10675,#10676,#10677,#10678,#10679,#10680,#10681,
#10682,#10683,#10684,#10685,#10686,#10687,#10688,#10689,#10690,#10691,#10692,
#10693,#10694,#10695,#10696,#10697,#10698,#10699,#10700,#10701,#10702,#10703,
#10704,#10705),(#10706,#10707,#10708,#10709,#10710,#10711,#10712,#10713,
#10714,#10715,#10716,#10717,#10718,#10719,#10720,#10721,#10722,#10723,#10724,
#10725,#10726,#10727,#10728,#10729,#10730,#10731,#10732,#10733,#10734,#10735,
#10736,#10737,#10738,#10739,#10740,#10741,#10742,#10743,#10744,#10745,#10746,
#10747,#10748,#10749,#10750,#10751,#10752,#10753,#10754,#10755,#10756,#10757,
#10758,#10759,#10760,#10761,#10762,#10763,#10764,#10765,#10766,#10767,#10768,
#10769,#10770,#10771,#10772,#10773,#10774,#10775,#10776,#10777,#10778,#10779,
#10780,#10781,#10782,#10783,#10784,#10785,#10786,#10787,#10788,#10789,#10790,
#10791,#10792,#10793,#10794,#10795,#10796,#10797,#10798,#10799,#10800,#10801,
#10802,#10803,#10804,#10805,#10806,#10807,#10808,#10809,#10810,#10811,#10812,
#10813,#10814,#10815,#10816,#10817,#10818,#10819,#10820,#10821,#10822,#10823,
#10824,#10825,#10826,#10827,#10828,#10829),(#10830,#10831,#10832,#10833,
#10834,#10835,#10836,#10837,#10838,#10839,#10840,#10841,#10842,#10843,#10844,
#10845,#10846,#10847,#10848,#10849,#10850,#10851,#10852,#10853,#10854,#10855,
#10856,#10857,#10858,#10859,#10860,#10861,#10862,#10863,#10864,#10865,#10866,
#10867,#10868,#10869,#10870,#10871,#10872,#10873,#10874,#10875,#10876,#10877,
#10878,#10879,#10880,#10881,#10882,#10883,#10884,#10885,#10886,#10887,#10888,
#10889,#10890,#10891,#10892,#10893,#10894,#10895,#10896,#10897,#10898,#10899,
#10900,#10901,#10902,#10903,#10904,#10905,#10906,#10907,#10908,#10909,#10910,
#10911,#10912,#10913,#10914,#10915,#10916,#10917,#10918,#10919,#10920,#10921,
#10922,#10923,#10924,#10925,#10926,#10927,#10928,#10929,#10930,#10931,#10932,
#10933,#10934,#10935,#10936,#10937,#10938,#10939,#10940,#10941,#10942,#10943,
#10944,#10945,#10946,#10947,#10948,#10949,#10950,#10951,#10952,#10953),
(#10954,#10955,#10956,#10957,#10958,#10959,#10960,#10961,#10962,#10963,
#10964,#10965,#10966,#10967,#10968,#10969,#10970,#10971,#10972,#10973,#10974,
#10975,#10976,#10977,#10978,#10979,#10980,#10981,#10982,#10983,#10984,#10985,
#10986,#10987,#10988,#10989,#10990,#10991,#10992,#10993,#10994,#10995,#10996,
#10997,#10998,#10999,#11000,#11001,#11002,#11003,#11004,#11005,#11006,#11007,
#11008,#11009,#11010,#11011,#11012,#11013,#11014,#11015,#11016,#11017,#11018,
#11019,#11020,#11021,#11022,#11023,#11024,#11025,#11026,#11027,#11028,#11029,
#11030,#11031,#11032,#11033,#11034,#11035,#11036,#11037,#11038,#11039,#11040,
#11041,#11042,#11043,#11044,#11045,#11046,#11047,#11048,#11049,#11050,#11051,
#11052,#11053,#11054,#11055,#11056,#11057,#11058,#11059,#11060,#11061,#11062,
#11063,#11064,#11065,#11066,#11067,#11068,#11069,#11070,#11071,#11072,#11073,
#11074,#11075,#11076,#11077),(#11078,#11079,#11080,#11081,#11082,#11083,
#11084,#11085,#11086,#11087,#11088,#11089,#11090,#11091,#11092,#11093,#11094,
#11095,#11096,#11097,#11098,#11099,#11100,#11101,#11102,#11103,#11104,#11105,
#11106,#11107,#11108,#11109,#11110,#11111,#11112,#11113,#11114,#11115,#11116,
#11117,#11118,#11119,#11120,#11121,#11122,#11123,#11124,#11125,#11126,#11127,
#11128,#11129,#11130,#11131,#11132,#11133,#11134,#11135,#11136,#11137,#11138,
#11139,#11140,#11141,#11142,#11143,#11144,#11145,#11146,#11147,#11148,#11149,
#11150,#11151,#11152,#11153,#11154,#11155,#11156,#11157,#11158,#11159,#11160,
#11161,#11162,#11163,#11164,#11165,#11166,#11167,#11168,#11169,#11170,#11171,
#11172,#11173,#11174,#11175,#11176,#11177,#11178,#11179,#11180,#11181,#11182,
#11183,#11184,#11185,#11186,#11187,#11188,#11189,#11190,#11191,#11192,#11193,
#11194,#11195,#11196,#11197,#11198,#11199,#11200,#11201),(#11202,#11203,
#11204,#11205,#11206,#11207,#11208,#11209,#11210,#11211,#11212,#11213,#11214,
#11215,#11216,#11217,#11218,#11219,#11220,#11221,#11222,#11223,#11224,#11225,
#11226,#11227,#11228,#11229,#11230,#11231,#11232,#11233,#11234,#11235,#11236,
#11237,#11238,#11239,#11240,#11241,#11242,#11243,#11244,#11245,#11246,#11247,
#11248,#11249,#11250,#11251,#11252,#11253,#11254,#11255,#11256,#11257,#11258,
#11259,#11260,#11261,#11262,#11263,#11264,#11265,#11266,#11267,#11268,#11269,
#11270,#11271,#11272,#11273,#11274,#11275,#11276,#11277,#11278,#11279,#11280,
#11281,#11282,#11283,#11284,#11285,#11286,#11287,#11288,#11289,#11290,#11291,
#11292,#11293,#11294,#11295,#11296,#11297,#11298,#11299,#11300,#11301,#11302,
#11303,#11304,#11305,#11306,#11307,#11308,#11309,#11310,#11311,#11312,#11313,
#11314,#11315,#11316,#11317,#11318,#11319,#11320,#11321,#11322,#11323,#11324,
#11325),(#11326,#11327,#11328,#11329,#11330,#11331,#11332,#11333,#11334,
#11335,#11336,#11337,#11338,#11339,#11340,#11341,#11342,#11343,#11344,#11345,
#11346,#11347,#11348,#11349,#11350,#11351,#11352,#11353,#11354,#11355,#11356,
#11357,#11358,#11359,#11360,#11361,#11362,#11363,#11364,#11365,#11366,#11367,
#11368,#11369,#11370,#11371,#11372,#11373,#11374,#11375,#11376,#11377,#11378,
#11379,#11380,#11381,#11382,#11383,#11384,#11385,#11386,#11387,#11388,#11389,
#11390,#11391,#11392,#11393,#11394,#11395,#11396,#11397,#11398,#11399,#11400,
#11401,#11402,#11403,#11404,#11405,#11406,#11407,#11408,#11409,#11410,#11411,
#11412,#11413,#11414,#11415,#11416,#11417,#11418,#11419,#11420,#11421,#11422,
#11423,#11424,#11425,#11426,#11427,#11428,#11429,#11430,#11431,#11432,#11433,
#11434,#11435,#11436,#11437,#11438,#11439,#11440,#11441,#11442,#11443,#11444,
#11445,#11446,#11447,#11448,#11449),(#11450,#11451,#11452,#11453,#11454,
#11455,#11456,#11457,#11458,#11459,#11460,#11461,#11462,#11463,#11464,#11465,
#11466,#11467,#11468,#11469,#11470,#11471,#11472,#11473,#11474,#11475,#11476,
#11477,#11478,#11479,#11480,#11481,#11482,#11483,#11484,#11485,#11486,#11487,
#11488,#11489,#11490,#11491,#11492,#11493,#11494,#11495,#11496,#11497,#11498,
#11499,#11500,#11501,#11502,#11503,#11504,#11505,#11506,#11507,#11508,#11509,
#11510,#11511,#11512,#11513,#11514,#11515,#11516,#11517,#11518,#11519,#11520,
#11521,#11522,#11523,#11524,#11525,#11526,#11527,#11528,#11529,#11530,#11531,
#11532,#11533,#11534,#11535,#11536,#11537,#11538,#11539,#11540,#11541,#11542,
#11543,#11544,#11545,#11546,#11547,#11548,#11549,#11550,#11551,#11552,#11553,
#11554,#11555,#11556,#11557,#11558,#11559,#11560,#11561,#11562,#11563,#11564,
#11565,#11566,#11567,#11568,#11569,#11570,#11571,#11572,#11573),(#11574,
#11575,#11576,#11577,#11578,#11579,#11580,#11581,#11582,#11583,#11584,#11585,
#11586,#11587,#11588,#11589,#11590,#11591,#11592,#11593,#11594,#11595,#11596,
#11597,#11598,#11599,#11600,#11601,#11602,#11603,#11604,#11605,#11606,#11607,
#11608,#11609,#11610,#11611,#11612,#11613,#11614,#11615,#11616,#11617,#11618,
#11619,#11620,#11621,#11622,#11623,#11624,#11625,#11626,#11627,#11628,#11629,
#11630,#11631,#11632,#11633,#11634,#11635,#11636,#11637,#11638,#11639,#11640,
#11641,#11642,#11643,#11644,#11645,#11646,#11647,#11648,#11649,#11650,#11651,
#11652,#11653,#11654,#11655,#11656,#11657,#11658,#11659,#11660,#11661,#11662,
#11663,#11664,#11665,#11666,#11667,#11668,#11669,#11670,#11671,#11672,#11673,
#11674,#11675,#11676,#11677,#11678,#11679,#11680,#11681,#11682,#11683,#11684,
#11685,#11686,#11687,#11688,#11689,#11690,#11691,#11692,#11693,#11694,#11695,
#11696,#11697)),.UNSPECIFIED.,.T.,.F.,.F.,(4,1,1,1,1,1,1,4),(4,1,1,1,1,
1,1,1,1,1,1,1,1,1,1,1,1,1,1,1,1,1,1,1,1,1,1,1,1,1,1,1,1,1,1,1,1,1,1,1,1,
1,1,1,1,1,1,1,1,1,1,1,1,1,1,1,1,1,1,1,1,1,1,1,1,1,1,1,1,1,1,1,1,1,1,1,1,
1,1,1,1,1,1,1,1,1,1,1,1,1,1,1,1,1,1,1,1,1,1,1,1,1,1,1,1,1,1,1,1,1,1,1,1,
1,1,1,1,1,1,1,1,4),(-3.14159265358979,-2.24399475256414,-1.34639685153848,
-0.448798950512828,0.448798950512828,1.34639685153848,2.24399475256414,
3.14159265358979),(0.,0.00892857142857143,0.0178571428571429,0.0267857142857143,
0.0357142857142857,0.0446428571428571,0.0535714285714286,0.0625,0.0714285714285714,
0.0803571428571428,0.0892857142857143,0.0982142857142857,0.107142857142857,
0.116071428571429,0.125,0.133928571428571,0.142857142857143,0.150793650793651,
0.154761904761905,0.156746031746032,0.158730158730159,0.166666666666667,
0.174603174603175,0.182539682539683,0.19047619047619,0.202380952380952,
0.214285714285714,0.222222222222222,0.23015873015873,0.238095238095238,
0.244047619047619,0.25,0.261904761904762,0.273809523809524,0.285714285714286,
0.297619047619048,0.30952380952381,0.321428571428571,0.327380952380952,
0.333333333333333,0.341269841269841,0.349206349206349,0.357142857142857,
0.365079365079365,0.373015873015873,0.380952380952381,0.386904761904762,
0.392857142857143,0.404761904761905,0.416666666666667,0.422619047619048,
0.428571428571429,0.4375,0.446428571428571,0.455357142857143,0.464285714285714,
0.468253968253968,0.476190476190476,0.482142857142857,0.488095238095238,
0.494047619047619,0.5,0.504464285714286,0.508928571428571,0.517857142857143,
0.526785714285714,0.535714285714286,0.540178571428571,0.544642857142857,
0.553571428571429,0.5625,0.571428571428571,0.580357142857143,0.589285714285714,
0.598214285714286,0.607142857142857,0.616071428571429,0.625,0.633928571428571,
0.642857142857143,0.650793650793651,0.658730158730159,0.666666666666667,
0.672619047619048,0.678571428571428,0.69047619047619,0.696428571428571,
0.702380952380952,0.714285714285714,0.726190476190476,0.738095238095238,
0.746031746031746,0.753968253968254,0.761904761904762,0.76984126984127,
0.777777777777778,0.785714285714286,0.790178571428571,0.794642857142857,
0.803571428571428,0.8125,0.821428571428571,0.830357142857143,0.839285714285714,
0.848214285714286,0.857142857142857,0.866071428571429,0.875,0.883928571428571,
0.892857142857143,0.901785714285714,0.910714285714286,0.919642857142857,
0.928571428571429,0.9375,0.946428571428571,0.955357142857143,0.964285714285714,
0.973214285714286,0.982142857142857,0.991071428571429,1.),.UNSPECIFIED.);
#348=SHAPE_REPRESENTATION_RELATIONSHIP('SRR','None',#13441,#385);
#349=SHAPE_REPRESENTATION_RELATIONSHIP('SRR','None',#13442,#386);
#350=SHAPE_REPRESENTATION_RELATIONSHIP('SRR','None',#13443,#387);
#351=SHAPE_REPRESENTATION_RELATIONSHIP('SRR','None',#13444,#388);
#352=SHAPE_REPRESENTATION_RELATIONSHIP('SRR','None',#13445,#389);
#353=SHAPE_REPRESENTATION_RELATIONSHIP('SRR','None',#13446,#390);
#354=SHAPE_REPRESENTATION_RELATIONSHIP('SRR','None',#13447,#391);
#355=SHAPE_REPRESENTATION_RELATIONSHIP('SRR','None',#13448,#392);
#356=SHAPE_REPRESENTATION_RELATIONSHIP('SRR','None',#13449,#393);
#357=SHAPE_REPRESENTATION_RELATIONSHIP('SRR','None',#13450,#394);
#358=SHAPE_REPRESENTATION_RELATIONSHIP('SRR','None',#13451,#395);
#359=SHAPE_REPRESENTATION_RELATIONSHIP('SRR','None',#13452,#396);
#360=SHAPE_REPRESENTATION_RELATIONSHIP('SRR','None',#13453,#397);
#361=SHAPE_REPRESENTATION_RELATIONSHIP('SRR','None',#13455,#398);
#362=SHAPE_REPRESENTATION_RELATIONSHIP('SRR','None',#13456,#399);
#363=SHAPE_REPRESENTATION_RELATIONSHIP('SRR','None',#13457,#400);
#364=SHAPE_REPRESENTATION_RELATIONSHIP('SRR','None',#13458,#401);
#365=SHAPE_REPRESENTATION_RELATIONSHIP('SRR','None',#13459,#402);
#366=SHAPE_REPRESENTATION_RELATIONSHIP('SRR','None',#13460,#403);
#367=SHAPE_REPRESENTATION_RELATIONSHIP('SRR','None',#13462,#404);
#368=SHAPE_REPRESENTATION_RELATIONSHIP('SRR','None',#13463,#405);
#369=SHAPE_REPRESENTATION_RELATIONSHIP('SRR','None',#13464,#406);
#370=SHAPE_REPRESENTATION_RELATIONSHIP('SRR','None',#13466,#407);
#371=SHAPE_REPRESENTATION_RELATIONSHIP('SRR','None',#13467,#408);
#372=SHAPE_REPRESENTATION_RELATIONSHIP('SRR','None',#13468,#409);
#373=SHAPE_REPRESENTATION_RELATIONSHIP('SRR','None',#13469,#410);
#374=SHAPE_REPRESENTATION_RELATIONSHIP('SRR','None',#13470,#411);
#375=SHAPE_REPRESENTATION_RELATIONSHIP('SRR','None',#13471,#412);
#376=SHAPE_REPRESENTATION_RELATIONSHIP('SRR','None',#13472,#413);
#377=SHAPE_REPRESENTATION_RELATIONSHIP('SRR','None',#13473,#414);
#378=SHAPE_REPRESENTATION_RELATIONSHIP('SRR','None',#13474,#415);
#379=SHAPE_REPRESENTATION_RELATIONSHIP('SRR','None',#13475,#416);
#380=SHAPE_REPRESENTATION_RELATIONSHIP('SRR','None',#13476,#417);
#381=SHAPE_REPRESENTATION_RELATIONSHIP('SRR','None',#13477,#418);
#382=SHAPE_REPRESENTATION_RELATIONSHIP('SRR','None',#13479,#419);
#383=SHAPE_REPRESENTATION_RELATIONSHIP('SRR','None',#13480,#420);
#384=SHAPE_REPRESENTATION_RELATIONSHIP('SRR','None',#13481,#421);
#385=ADVANCED_BREP_SHAPE_REPRESENTATION('',(#466),#13236);
#386=ADVANCED_BREP_SHAPE_REPRESENTATION('',(#467),#13237);
#387=ADVANCED_BREP_SHAPE_REPRESENTATION('',(#468),#13238);
#388=ADVANCED_BREP_SHAPE_REPRESENTATION('',(#469),#13239);
#389=ADVANCED_BREP_SHAPE_REPRESENTATION('',(#470),#13240);
#390=ADVANCED_BREP_SHAPE_REPRESENTATION('',(#471),#13241);
#391=ADVANCED_BREP_SHAPE_REPRESENTATION('',(#472),#13242);
#392=ADVANCED_BREP_SHAPE_REPRESENTATION('',(#473),#13243);
#393=ADVANCED_BREP_SHAPE_REPRESENTATION('',(#474),#13244);
#394=ADVANCED_BREP_SHAPE_REPRESENTATION('',(#475),#13245);
#395=ADVANCED_BREP_SHAPE_REPRESENTATION('',(#476),#13246);
#396=ADVANCED_BREP_SHAPE_REPRESENTATION('',(#477),#13247);
#397=ADVANCED_BREP_SHAPE_REPRESENTATION('',(#478),#13248);
#398=ADVANCED_BREP_SHAPE_REPRESENTATION('',(#479),#13250);
#399=ADVANCED_BREP_SHAPE_REPRESENTATION('',(#480),#13251);
#400=ADVANCED_BREP_SHAPE_REPRESENTATION('',(#481,#482,#483,#484,#485,#486,
#487),#13252);
#401=ADVANCED_BREP_SHAPE_REPRESENTATION('',(#488),#13253);
#402=ADVANCED_BREP_SHAPE_REPRESENTATION('',(#489,#490),#13254);
#403=ADVANCED_BREP_SHAPE_REPRESENTATION('',(#14),#13255);
#404=ADVANCED_BREP_SHAPE_REPRESENTATION('',(#491),#13257);
#405=ADVANCED_BREP_SHAPE_REPRESENTATION('',(#492),#13258);
#406=ADVANCED_BREP_SHAPE_REPRESENTATION('',(#15),#13259);
#407=ADVANCED_BREP_SHAPE_REPRESENTATION('',(#493),#13261);
#408=ADVANCED_BREP_SHAPE_REPRESENTATION('',(#494),#13262);
#409=ADVANCED_BREP_SHAPE_REPRESENTATION('',(#495),#13263);
#410=ADVANCED_BREP_SHAPE_REPRESENTATION('',(#496),#13264);
#411=ADVANCED_BREP_SHAPE_REPRESENTATION('',(#497),#13265);
#412=ADVANCED_BREP_SHAPE_REPRESENTATION('',(#498),#13266);
#413=ADVANCED_BREP_SHAPE_REPRESENTATION('',(#499),#13267);
#414=ADVANCED_BREP_SHAPE_REPRESENTATION('',(#500),#13268);
#415=ADVANCED_BREP_SHAPE_REPRESENTATION('',(#501),#13269);
#416=ADVANCED_BREP_SHAPE_REPRESENTATION('',(#502),#13270);
#417=ADVANCED_BREP_SHAPE_REPRESENTATION('',(#503),#13271);
#418=ADVANCED_BREP_SHAPE_REPRESENTATION('',(#16),#13272);
#419=ADVANCED_BREP_SHAPE_REPRESENTATION('',(#504),#13274);
#420=ADVANCED_BREP_SHAPE_REPRESENTATION('',(#505),#13275);
#421=ADVANCED_BREP_SHAPE_REPRESENTATION('',(#506),#13276);
#422=STYLED_ITEM('',(#13699),#466);
#423=STYLED_ITEM('',(#13734),#467);
#424=STYLED_ITEM('',(#13734),#468);
#425=STYLED_ITEM('',(#13720),#469);
#426=STYLED_ITEM('',(#13720),#470);
#427=STYLED_ITEM('',(#13720),#471);
#428=STYLED_ITEM('',(#13720),#472);
#429=STYLED_ITEM('',(#13720),#473);
#430=STYLED_ITEM('',(#13720),#474);
#431=STYLED_ITEM('',(#13713),#475);
#432=STYLED_ITEM('',(#13706),#476);
#433=STYLED_ITEM('',(#13734),#477);
#434=STYLED_ITEM('',(#13720),#478);
#435=STYLED_ITEM('',(#13720),#479);
#436=STYLED_ITEM('',(#13720),#480);
#437=STYLED_ITEM('',(#13720),#481);
#438=STYLED_ITEM('',(#13720),#482);
#439=STYLED_ITEM('',(#13720),#483);
#440=STYLED_ITEM('',(#13720),#484);
#441=STYLED_ITEM('',(#13720),#485);
#442=STYLED_ITEM('',(#13720),#486);
#443=STYLED_ITEM('',(#13720),#487);
#444=STYLED_ITEM('',(#13720),#488);
#445=STYLED_ITEM('',(#13720),#489);
#446=STYLED_ITEM('',(#13720),#490);
#447=STYLED_ITEM('',(#13727),#14);
#448=STYLED_ITEM('',(#13734),#491);
#449=STYLED_ITEM('',(#13713),#492);
#450=STYLED_ITEM('',(#13727),#15);
#451=STYLED_ITEM('',(#13720),#493);
#452=STYLED_ITEM('',(#13720),#494);
#453=STYLED_ITEM('',(#13720),#495);
#454=STYLED_ITEM('',(#13720),#496);
#455=STYLED_ITEM('',(#13720),#497);
#456=STYLED_ITEM('',(#13734),#498);
#457=STYLED_ITEM('',(#13706),#499);
#458=STYLED_ITEM('',(#13727),#500);
#459=STYLED_ITEM('',(#13706),#501);
#460=STYLED_ITEM('',(#13706),#502);
#461=STYLED_ITEM('',(#13720),#503);
#462=STYLED_ITEM('',(#13727),#16);
#463=STYLED_ITEM('',(#13706),#504);
#464=STYLED_ITEM('',(#13706),#505);
#465=STYLED_ITEM('',(#13727),#506);
#466=MANIFOLD_SOLID_BREP('Body1',#6398);
#467=MANIFOLD_SOLID_BREP('Body1',#6399);
#468=MANIFOLD_SOLID_BREP('Body1',#6400);
#469=MANIFOLD_SOLID_BREP('Body1',#6401);
#470=MANIFOLD_SOLID_BREP('Body1',#6402);
#471=MANIFOLD_SOLID_BREP('Body1',#6403);
#472=MANIFOLD_SOLID_BREP('Body1',#6404);
#473=MANIFOLD_SOLID_BREP('Body1',#6405);
#474=MANIFOLD_SOLID_BREP('Body1',#6406);
#475=MANIFOLD_SOLID_BREP('Body1',#6407);
#476=MANIFOLD_SOLID_BREP('Body1',#6408);
#477=MANIFOLD_SOLID_BREP('Body1',#6409);
#478=MANIFOLD_SOLID_BREP('Body1',#6410);
#479=MANIFOLD_SOLID_BREP('Body1',#6411);
#480=MANIFOLD_SOLID_BREP('Body1',#6412);
#481=MANIFOLD_SOLID_BREP('Body1',#6413);
#482=MANIFOLD_SOLID_BREP('Body2',#6414);
#483=MANIFOLD_SOLID_BREP('Body3',#6415);
#484=MANIFOLD_SOLID_BREP('Body4',#6416);
#485=MANIFOLD_SOLID_BREP('Body5',#6417);
#486=MANIFOLD_SOLID_BREP('Body6',#6418);
#487=MANIFOLD_SOLID_BREP('Body7',#6419);
#488=MANIFOLD_SOLID_BREP('Continuous crown cage',#6420);
#489=MANIFOLD_SOLID_BREP('Body1',#6421);
#490=MANIFOLD_SOLID_BREP('Body2',#6422);
#491=MANIFOLD_SOLID_BREP('Body1',#6425);
#492=MANIFOLD_SOLID_BREP('Body1',#6426);
#493=MANIFOLD_SOLID_BREP('Body1',#6429);
#494=MANIFOLD_SOLID_BREP('Body1',#6430);
#495=MANIFOLD_SOLID_BREP('Body1',#6431);
#496=MANIFOLD_SOLID_BREP('Body1',#6432);
#497=MANIFOLD_SOLID_BREP('Body1',#6433);
#498=MANIFOLD_SOLID_BREP('Body2',#6434);
#499=MANIFOLD_SOLID_BREP('Body1',#6435);
#500=MANIFOLD_SOLID_BREP('Body1',#6436);
#501=MANIFOLD_SOLID_BREP('Body1',#6437);
#502=MANIFOLD_SOLID_BREP('Body1',#6438);
#503=MANIFOLD_SOLID_BREP('Body1',#6439);
#504=MANIFOLD_SOLID_BREP('Body1',#6442);
#505=MANIFOLD_SOLID_BREP('Body1',#6443);
#506=MANIFOLD_SOLID_BREP('Body1',#6444);
#507=FACE_BOUND('',#1296,.T.);
#508=FACE_BOUND('',#1297,.T.);
#509=FACE_BOUND('',#1298,.T.);
#510=FACE_BOUND('',#1299,.T.);
#511=FACE_BOUND('',#1300,.T.);
#512=FACE_BOUND('',#1301,.T.);
#513=FACE_BOUND('',#1302,.T.);
#514=FACE_BOUND('',#1304,.T.);
#515=FACE_BOUND('',#1305,.T.);
#516=FACE_BOUND('',#1306,.T.);
#517=FACE_BOUND('',#1307,.T.);
#518=FACE_BOUND('',#1308,.T.);
#519=FACE_BOUND('',#1309,.T.);
#520=FACE_BOUND('',#1330,.T.);
#521=FACE_BOUND('',#1332,.T.);
#522=FACE_BOUND('',#1336,.T.);
#523=FACE_BOUND('',#1337,.T.);
#524=FACE_BOUND('',#1338,.T.);
#525=FACE_BOUND('',#1339,.T.);
#526=FACE_BOUND('',#1340,.T.);
#527=FACE_BOUND('',#1343,.T.);
#528=FACE_BOUND('',#1344,.T.);
#529=FACE_BOUND('',#1345,.T.);
#530=FACE_BOUND('',#1346,.T.);
#531=FACE_BOUND('',#1347,.T.);
#532=FACE_BOUND('',#1351,.T.);
#533=FACE_BOUND('',#1352,.T.);
#534=FACE_BOUND('',#1359,.T.);
#535=FACE_BOUND('',#1363,.T.);
#536=FACE_BOUND('',#1364,.T.);
#537=FACE_BOUND('',#1365,.T.);
#538=FACE_BOUND('',#1366,.T.);
#539=FACE_BOUND('',#1367,.T.);
#540=FACE_BOUND('',#1369,.T.);
#541=FACE_BOUND('',#1370,.T.);
#542=FACE_BOUND('',#1371,.T.);
#543=FACE_BOUND('',#1372,.T.);
#544=FACE_BOUND('',#1373,.T.);
#545=FACE_BOUND('',#1380,.T.);
#546=FACE_BOUND('',#1384,.T.);
#547=FACE_BOUND('',#1385,.T.);
#548=FACE_BOUND('',#1386,.T.);
#549=FACE_BOUND('',#1387,.T.);
#550=FACE_BOUND('',#1388,.T.);
#551=FACE_BOUND('',#1390,.T.);
#552=FACE_BOUND('',#1391,.T.);
#553=FACE_BOUND('',#1392,.T.);
#554=FACE_BOUND('',#1393,.T.);
#555=FACE_BOUND('',#1394,.T.);
#556=FACE_BOUND('',#1403,.T.);
#557=FACE_BOUND('',#1405,.T.);
#558=FACE_BOUND('',#1409,.T.);
#559=FACE_BOUND('',#1410,.T.);
#560=FACE_BOUND('',#1411,.T.);
#561=FACE_BOUND('',#1412,.T.);
#562=FACE_BOUND('',#1413,.T.);
#563=FACE_BOUND('',#1416,.T.);
#564=FACE_BOUND('',#1417,.T.);
#565=FACE_BOUND('',#1418,.T.);
#566=FACE_BOUND('',#1419,.T.);
#567=FACE_BOUND('',#1420,.T.);
#568=FACE_BOUND('',#1424,.T.);
#569=FACE_BOUND('',#1425,.T.);
#570=FACE_BOUND('',#1432,.T.);
#571=FACE_BOUND('',#1436,.T.);
#572=FACE_BOUND('',#1437,.T.);
#573=FACE_BOUND('',#1438,.T.);
#574=FACE_BOUND('',#1439,.T.);
#575=FACE_BOUND('',#1440,.T.);
#576=FACE_BOUND('',#1442,.T.);
#577=FACE_BOUND('',#1443,.T.);
#578=FACE_BOUND('',#1444,.T.);
#579=FACE_BOUND('',#1445,.T.);
#580=FACE_BOUND('',#1446,.T.);
#581=FACE_BOUND('',#1453,.T.);
#582=FACE_BOUND('',#1457,.T.);
#583=FACE_BOUND('',#1458,.T.);
#584=FACE_BOUND('',#1459,.T.);
#585=FACE_BOUND('',#1460,.T.);
#586=FACE_BOUND('',#1461,.T.);
#587=FACE_BOUND('',#1463,.T.);
#588=FACE_BOUND('',#1464,.T.);
#589=FACE_BOUND('',#1465,.T.);
#590=FACE_BOUND('',#1466,.T.);
#591=FACE_BOUND('',#1467,.T.);
#592=FACE_BOUND('',#1478,.T.);
#593=FACE_BOUND('',#1482,.T.);
#594=FACE_BOUND('',#1486,.T.);
#595=FACE_BOUND('',#1489,.T.);
#596=FACE_BOUND('',#1495,.T.);
#597=FACE_BOUND('',#1503,.T.);
#598=FACE_BOUND('',#1504,.T.);
#599=FACE_BOUND('',#1505,.T.);
#600=FACE_BOUND('',#1506,.T.);
#601=FACE_BOUND('',#1507,.T.);
#602=FACE_BOUND('',#1508,.T.);
#603=FACE_BOUND('',#1509,.T.);
#604=FACE_BOUND('',#1511,.T.);
#605=FACE_BOUND('',#1515,.T.);
#606=FACE_BOUND('',#1517,.T.);
#607=FACE_BOUND('',#1524,.T.);
#608=FACE_BOUND('',#1528,.T.);
#609=FACE_BOUND('',#1529,.T.);
#610=FACE_BOUND('',#1530,.T.);
#611=FACE_BOUND('',#1531,.T.);
#612=FACE_BOUND('',#1532,.T.);
#613=FACE_BOUND('',#1534,.T.);
#614=FACE_BOUND('',#1535,.T.);
#615=FACE_BOUND('',#1536,.T.);
#616=FACE_BOUND('',#1537,.T.);
#617=FACE_BOUND('',#1538,.T.);
#618=FACE_BOUND('',#1547,.T.);
#619=FACE_BOUND('',#1550,.T.);
#620=FACE_BOUND('',#1555,.T.);
#621=FACE_BOUND('',#1560,.T.);
#622=FACE_BOUND('',#1585,.T.);
#623=FACE_BOUND('',#1588,.T.);
#624=FACE_BOUND('',#1591,.T.);
#625=FACE_BOUND('',#1594,.T.);
#626=FACE_BOUND('',#1597,.T.);
#627=FACE_BOUND('',#1604,.T.);
#628=FACE_BOUND('',#1623,.T.);
#629=FACE_BOUND('',#1626,.T.);
#630=FACE_BOUND('',#1629,.T.);
#631=FACE_BOUND('',#1632,.T.);
#632=FACE_BOUND('',#1635,.T.);
#633=FACE_BOUND('',#1638,.T.);
#634=FACE_BOUND('',#1640,.T.);
#635=FACE_BOUND('',#1646,.T.);
#636=FACE_BOUND('',#1648,.T.);
#637=FACE_BOUND('',#1650,.T.);
#638=FACE_BOUND('',#1652,.T.);
#639=FACE_BOUND('',#1667,.T.);
#640=FACE_BOUND('',#1685,.T.);
#641=FACE_BOUND('',#1686,.T.);
#642=FACE_BOUND('',#1688,.T.);
#643=FACE_BOUND('',#1690,.T.);
#644=FACE_BOUND('',#1694,.T.);
#645=FACE_BOUND('',#1696,.T.);
#646=FACE_BOUND('',#1700,.T.);
#647=FACE_BOUND('',#1702,.T.);
#648=FACE_BOUND('',#1706,.T.);
#649=FACE_BOUND('',#1708,.T.);
#650=FACE_BOUND('',#1712,.T.);
#651=FACE_BOUND('',#1714,.T.);
#652=FACE_BOUND('',#1719,.T.);
#653=FACE_BOUND('',#1724,.T.);
#654=FACE_BOUND('',#1727,.T.);
#655=FACE_BOUND('',#1729,.T.);
#656=FACE_BOUND('',#1735,.T.);
#657=FACE_BOUND('',#1739,.T.);
#658=FACE_BOUND('',#1743,.T.);
#659=FACE_BOUND('',#1745,.T.);
#660=FACE_BOUND('',#1747,.T.);
#661=FACE_BOUND('',#1753,.T.);
#662=FACE_BOUND('',#1757,.T.);
#663=FACE_BOUND('',#1759,.T.);
#664=FACE_BOUND('',#1763,.T.);
#665=FACE_BOUND('',#1765,.T.);
#666=FACE_BOUND('',#1781,.T.);
#667=FACE_BOUND('',#1800,.T.);
#668=FACE_BOUND('',#1802,.T.);
#669=FACE_BOUND('',#1808,.T.);
#670=FACE_BOUND('',#1809,.T.);
#671=FACE_BOUND('',#1810,.T.);
#672=FACE_BOUND('',#1811,.T.);
#673=FACE_BOUND('',#1812,.T.);
#674=FACE_BOUND('',#1818,.T.);
#675=FACE_BOUND('',#1819,.T.);
#676=FACE_BOUND('',#1820,.T.);
#677=FACE_BOUND('',#1821,.T.);
#678=FACE_BOUND('',#1826,.T.);
#679=FACE_BOUND('',#1830,.T.);
#680=FACE_BOUND('',#1832,.T.);
#681=PLANE('',#6874);
#682=PLANE('',#6875);
#683=PLANE('',#6876);
#684=PLANE('',#6877);
#685=PLANE('',#6878);
#686=PLANE('',#6879);
#687=PLANE('',#6880);
#688=PLANE('',#6881);
#689=PLANE('',#6882);
#690=PLANE('',#6883);
#691=PLANE('',#6884);
#692=PLANE('',#6886);
#693=PLANE('',#6887);
#694=PLANE('',#6888);
#695=PLANE('',#6889);
#696=PLANE('',#6890);
#697=PLANE('',#6891);
#698=PLANE('',#6893);
#699=PLANE('',#6894);
#700=PLANE('',#6895);
#701=PLANE('',#6896);
#702=PLANE('',#6897);
#703=PLANE('',#6898);
#704=PLANE('',#6921);
#705=PLANE('',#6922);
#706=PLANE('',#6923);
#707=PLANE('',#6924);
#708=PLANE('',#6925);
#709=PLANE('',#6926);
#710=PLANE('',#6927);
#711=PLANE('',#6928);
#712=PLANE('',#6929);
#713=PLANE('',#6930);
#714=PLANE('',#6947);
#715=PLANE('',#6954);
#716=PLANE('',#6955);
#717=PLANE('',#6972);
#718=PLANE('',#6979);
#719=PLANE('',#6980);
#720=PLANE('',#7003);
#721=PLANE('',#7004);
#722=PLANE('',#7005);
#723=PLANE('',#7006);
#724=PLANE('',#7007);
#725=PLANE('',#7008);
#726=PLANE('',#7009);
#727=PLANE('',#7010);
#728=PLANE('',#7011);
#729=PLANE('',#7012);
#730=PLANE('',#7029);
#731=PLANE('',#7036);
#732=PLANE('',#7037);
#733=PLANE('',#7054);
#734=PLANE('',#7061);
#735=PLANE('',#7062);
#736=PLANE('',#7067);
#737=PLANE('',#7071);
#738=PLANE('',#7075);
#739=PLANE('',#7079);
#740=PLANE('',#7083);
#741=PLANE('',#7090);
#742=PLANE('',#7097);
#743=PLANE('',#7101);
#744=PLANE('',#7102);
#745=PLANE('',#7103);
#746=PLANE('',#7104);
#747=PLANE('',#7105);
#748=PLANE('',#7106);
#749=PLANE('',#7107);
#750=PLANE('',#7108);
#751=PLANE('',#7109);
#752=PLANE('',#7110);
#753=PLANE('',#7111);
#754=PLANE('',#7112);
#755=PLANE('',#7113);
#756=PLANE('',#7114);
#757=PLANE('',#7122);
#758=PLANE('',#7123);
#759=PLANE('',#7140);
#760=PLANE('',#7147);
#761=PLANE('',#7148);
#762=PLANE('',#7152);
#763=PLANE('',#7153);
#764=PLANE('',#7169);
#765=PLANE('',#7172);
#766=PLANE('',#7184);
#767=PLANE('',#7193);
#768=PLANE('',#7224);
#769=PLANE('',#7229);
#770=PLANE('',#7234);
#771=PLANE('',#7240);
#772=PLANE('',#7245);
#773=PLANE('',#7254);
#774=PLANE('',#7258);
#775=PLANE('',#7259);
#776=PLANE('',#7261);
#777=PLANE('',#7266);
#778=PLANE('',#7269);
#779=PLANE('',#7274);
#780=PLANE('',#7283);
#781=PLANE('',#7291);
#782=PLANE('',#7299);
#783=PLANE('',#7300);
#784=PLANE('',#7301);
#785=PLANE('',#7302);
#786=PLANE('',#7303);
#787=PLANE('',#7304);
#788=PLANE('',#7305);
#789=PLANE('',#7306);
#790=PLANE('',#7307);
#791=PLANE('',#7310);
#792=PLANE('',#7312);
#793=PLANE('',#7313);
#794=PLANE('',#7315);
#795=PLANE('',#7316);
#796=PLANE('',#7317);
#797=PLANE('',#7322);
#798=PLANE('',#7326);
#799=PLANE('',#7330);
#800=PLANE('',#7334);
#801=PLANE('',#7338);
#802=PLANE('',#7342);
#803=PLANE('',#7345);
#804=PLANE('',#7346);
#805=PLANE('',#7349);
#806=PLANE('',#7350);
#807=PLANE('',#7355);
#808=PLANE('',#7361);
#809=PLANE('',#7362);
#810=PLANE('',#7363);
#811=PLANE('',#7364);
#812=PLANE('',#7365);
#813=PLANE('',#7366);
#814=PLANE('',#7367);
#815=PLANE('',#7368);
#816=PLANE('',#7369);
#817=PLANE('',#7371);
#818=PLANE('',#7379);
#819=PLANE('',#7389);
#820=PLANE('',#7393);
#821=PLANE('',#7394);
#822=PLANE('',#7395);
#823=PLANE('',#7397);
#824=PLANE('',#7398);
#825=PLANE('',#7399);
#826=PLANE('',#7401);
#827=PLANE('',#7402);
#828=PLANE('',#7404);
#829=PLANE('',#7405);
#830=PLANE('',#7406);
#831=PLANE('',#7411);
#832=PLANE('',#7412);
#833=PLANE('',#7420);
#834=PLANE('',#7421);
#835=PLANE('',#7429);
#836=PLANE('',#7430);
#837=PLANE('',#7438);
#838=PLANE('',#7439);
#839=PLANE('',#7447);
#840=PLANE('',#7448);
#841=PLANE('',#7450);
#842=PLANE('',#7451);
#843=PLANE('',#7452);
#844=PLANE('',#7453);
#845=PLANE('',#7463);
#846=PLANE('',#7467);
#847=PLANE('',#7468);
#848=PLANE('',#7473);
#849=PLANE('',#7474);
#850=PLANE('',#7475);
#851=PLANE('',#7476);
#852=PLANE('',#7484);
#853=PLANE('',#7486);
#854=PLANE('',#7487);
#855=PLANE('',#7488);
#856=PLANE('',#7492);
#857=PLANE('',#7497);
#858=PLANE('',#7501);
#859=PLANE('',#7502);
#860=PLANE('',#7510);
#861=PLANE('',#7511);
#862=PLANE('',#7519);
#863=PLANE('',#7520);
#864=PLANE('',#7522);
#865=PLANE('',#7523);
#866=PLANE('',#7524);
#867=PLANE('',#7525);
#868=PLANE('',#7526);
#869=PLANE('',#7527);
#870=PLANE('',#7528);
#871=PLANE('',#7529);
#872=PLANE('',#7530);
#873=PLANE('',#7531);
#874=PLANE('',#7533);
#875=PLANE('',#7541);
#876=PLANE('',#7549);
#877=PLANE('',#7550);
#878=PLANE('',#7551);
#879=PLANE('',#7552);
#880=PLANE('',#7553);
#881=PLANE('',#7554);
#882=PLANE('',#7555);
#883=PLANE('',#7556);
#884=PLANE('',#7557);
#885=PLANE('',#7621);
#886=PLANE('',#7622);
#887=PLANE('',#7623);
#888=PLANE('',#7624);
#889=PLANE('',#7625);
#890=PLANE('',#7626);
#891=PLANE('',#7640);
#892=PLANE('',#7642);
#893=PLANE('',#7643);
#894=PLANE('',#7644);
#895=PLANE('',#7645);
#896=PLANE('',#7646);
#897=PLANE('',#7650);
#898=PLANE('',#7653);
#899=PLANE('',#7661);
#900=PLANE('',#7662);
#901=FACE_OUTER_BOUND('',#1280,.T.);
#902=FACE_OUTER_BOUND('',#1281,.T.);
#903=FACE_OUTER_BOUND('',#1282,.T.);
#904=FACE_OUTER_BOUND('',#1283,.T.);
#905=FACE_OUTER_BOUND('',#1284,.T.);
#906=FACE_OUTER_BOUND('',#1285,.T.);
#907=FACE_OUTER_BOUND('',#1286,.T.);
#908=FACE_OUTER_BOUND('',#1287,.T.);
#909=FACE_OUTER_BOUND('',#1288,.T.);
#910=FACE_OUTER_BOUND('',#1289,.T.);
#911=FACE_OUTER_BOUND('',#1290,.T.);
#912=FACE_OUTER_BOUND('',#1291,.T.);
#913=FACE_OUTER_BOUND('',#1292,.T.);
#914=FACE_OUTER_BOUND('',#1293,.T.);
#915=FACE_OUTER_BOUND('',#1294,.T.);
#916=FACE_OUTER_BOUND('',#1295,.T.);
#917=FACE_OUTER_BOUND('',#1303,.T.);
#918=FACE_OUTER_BOUND('',#1310,.T.);
#919=FACE_OUTER_BOUND('',#1311,.T.);
#920=FACE_OUTER_BOUND('',#1312,.T.);
#921=FACE_OUTER_BOUND('',#1313,.T.);
#922=FACE_OUTER_BOUND('',#1314,.T.);
#923=FACE_OUTER_BOUND('',#1315,.T.);
#924=FACE_OUTER_BOUND('',#1316,.T.);
#925=FACE_OUTER_BOUND('',#1317,.T.);
#926=FACE_OUTER_BOUND('',#1318,.T.);
#927=FACE_OUTER_BOUND('',#1319,.T.);
#928=FACE_OUTER_BOUND('',#1320,.T.);
#929=FACE_OUTER_BOUND('',#1321,.T.);
#930=FACE_OUTER_BOUND('',#1322,.T.);
#931=FACE_OUTER_BOUND('',#1323,.T.);
#932=FACE_OUTER_BOUND('',#1324,.T.);
#933=FACE_OUTER_BOUND('',#1325,.T.);
#934=FACE_OUTER_BOUND('',#1326,.T.);
#935=FACE_OUTER_BOUND('',#1327,.T.);
#936=FACE_OUTER_BOUND('',#1328,.T.);
#937=FACE_OUTER_BOUND('',#1329,.T.);
#938=FACE_OUTER_BOUND('',#1331,.T.);
#939=FACE_OUTER_BOUND('',#1333,.T.);
#940=FACE_OUTER_BOUND('',#1334,.T.);
#941=FACE_OUTER_BOUND('',#1335,.T.);
#942=FACE_OUTER_BOUND('',#1341,.T.);
#943=FACE_OUTER_BOUND('',#1342,.T.);
#944=FACE_OUTER_BOUND('',#1348,.T.);
#945=FACE_OUTER_BOUND('',#1349,.T.);
#946=FACE_OUTER_BOUND('',#1350,.T.);
#947=FACE_OUTER_BOUND('',#1353,.T.);
#948=FACE_OUTER_BOUND('',#1354,.T.);
#949=FACE_OUTER_BOUND('',#1355,.T.);
#950=FACE_OUTER_BOUND('',#1356,.T.);
#951=FACE_OUTER_BOUND('',#1357,.T.);
#952=FACE_OUTER_BOUND('',#1358,.T.);
#953=FACE_OUTER_BOUND('',#1360,.T.);
#954=FACE_OUTER_BOUND('',#1361,.T.);
#955=FACE_OUTER_BOUND('',#1362,.T.);
#956=FACE_OUTER_BOUND('',#1368,.T.);
#957=FACE_OUTER_BOUND('',#1374,.T.);
#958=FACE_OUTER_BOUND('',#1375,.T.);
#959=FACE_OUTER_BOUND('',#1376,.T.);
#960=FACE_OUTER_BOUND('',#1377,.T.);
#961=FACE_OUTER_BOUND('',#1378,.T.);
#962=FACE_OUTER_BOUND('',#1379,.T.);
#963=FACE_OUTER_BOUND('',#1381,.T.);
#964=FACE_OUTER_BOUND('',#1382,.T.);
#965=FACE_OUTER_BOUND('',#1383,.T.);
#966=FACE_OUTER_BOUND('',#1389,.T.);
#967=FACE_OUTER_BOUND('',#1395,.T.);
#968=FACE_OUTER_BOUND('',#1396,.T.);
#969=FACE_OUTER_BOUND('',#1397,.T.);
#970=FACE_OUTER_BOUND('',#1398,.T.);
#971=FACE_OUTER_BOUND('',#1399,.T.);
#972=FACE_OUTER_BOUND('',#1400,.T.);
#973=FACE_OUTER_BOUND('',#1401,.T.);
#974=FACE_OUTER_BOUND('',#1402,.T.);
#975=FACE_OUTER_BOUND('',#1404,.T.);
#976=FACE_OUTER_BOUND('',#1406,.T.);
#977=FACE_OUTER_BOUND('',#1407,.T.);
#978=FACE_OUTER_BOUND('',#1408,.T.);
#979=FACE_OUTER_BOUND('',#1414,.T.);
#980=FACE_OUTER_BOUND('',#1415,.T.);
#981=FACE_OUTER_BOUND('',#1421,.T.);
#982=FACE_OUTER_BOUND('',#1422,.T.);
#983=FACE_OUTER_BOUND('',#1423,.T.);
#984=FACE_OUTER_BOUND('',#1426,.T.);
#985=FACE_OUTER_BOUND('',#1427,.T.);
#986=FACE_OUTER_BOUND('',#1428,.T.);
#987=FACE_OUTER_BOUND('',#1429,.T.);
#988=FACE_OUTER_BOUND('',#1430,.T.);
#989=FACE_OUTER_BOUND('',#1431,.T.);
#990=FACE_OUTER_BOUND('',#1433,.T.);
#991=FACE_OUTER_BOUND('',#1434,.T.);
#992=FACE_OUTER_BOUND('',#1435,.T.);
#993=FACE_OUTER_BOUND('',#1441,.T.);
#994=FACE_OUTER_BOUND('',#1447,.T.);
#995=FACE_OUTER_BOUND('',#1448,.T.);
#996=FACE_OUTER_BOUND('',#1449,.T.);
#997=FACE_OUTER_BOUND('',#1450,.T.);
#998=FACE_OUTER_BOUND('',#1451,.T.);
#999=FACE_OUTER_BOUND('',#1452,.T.);
#1000=FACE_OUTER_BOUND('',#1454,.T.);
#1001=FACE_OUTER_BOUND('',#1455,.T.);
#1002=FACE_OUTER_BOUND('',#1456,.T.);
#1003=FACE_OUTER_BOUND('',#1462,.T.);
#1004=FACE_OUTER_BOUND('',#1468,.T.);
#1005=FACE_OUTER_BOUND('',#1469,.T.);
#1006=FACE_OUTER_BOUND('',#1470,.T.);
#1007=FACE_OUTER_BOUND('',#1471,.T.);
#1008=FACE_OUTER_BOUND('',#1472,.T.);
#1009=FACE_OUTER_BOUND('',#1473,.T.);
#1010=FACE_OUTER_BOUND('',#1474,.T.);
#1011=FACE_OUTER_BOUND('',#1475,.T.);
#1012=FACE_OUTER_BOUND('',#1476,.T.);
#1013=FACE_OUTER_BOUND('',#1477,.T.);
#1014=FACE_OUTER_BOUND('',#1479,.T.);
#1015=FACE_OUTER_BOUND('',#1480,.T.);
#1016=FACE_OUTER_BOUND('',#1481,.T.);
#1017=FACE_OUTER_BOUND('',#1483,.T.);
#1018=FACE_OUTER_BOUND('',#1484,.T.);
#1019=FACE_OUTER_BOUND('',#1485,.T.);
#1020=FACE_OUTER_BOUND('',#1487,.T.);
#1021=FACE_OUTER_BOUND('',#1488,.T.);
#1022=FACE_OUTER_BOUND('',#1490,.T.);
#1023=FACE_OUTER_BOUND('',#1491,.T.);
#1024=FACE_OUTER_BOUND('',#1492,.T.);
#1025=FACE_OUTER_BOUND('',#1493,.T.);
#1026=FACE_OUTER_BOUND('',#1494,.T.);
#1027=FACE_OUTER_BOUND('',#1496,.T.);
#1028=FACE_OUTER_BOUND('',#1497,.T.);
#1029=FACE_OUTER_BOUND('',#1498,.T.);
#1030=FACE_OUTER_BOUND('',#1499,.T.);
#1031=FACE_OUTER_BOUND('',#1500,.T.);
#1032=FACE_OUTER_BOUND('',#1501,.T.);
#1033=FACE_OUTER_BOUND('',#1502,.T.);
#1034=FACE_OUTER_BOUND('',#1510,.T.);
#1035=FACE_OUTER_BOUND('',#1512,.T.);
#1036=FACE_OUTER_BOUND('',#1513,.T.);
#1037=FACE_OUTER_BOUND('',#1514,.T.);
#1038=FACE_OUTER_BOUND('',#1516,.T.);
#1039=FACE_OUTER_BOUND('',#1518,.T.);
#1040=FACE_OUTER_BOUND('',#1519,.T.);
#1041=FACE_OUTER_BOUND('',#1520,.T.);
#1042=FACE_OUTER_BOUND('',#1521,.T.);
#1043=FACE_OUTER_BOUND('',#1522,.T.);
#1044=FACE_OUTER_BOUND('',#1523,.T.);
#1045=FACE_OUTER_BOUND('',#1525,.T.);
#1046=FACE_OUTER_BOUND('',#1526,.T.);
#1047=FACE_OUTER_BOUND('',#1527,.T.);
#1048=FACE_OUTER_BOUND('',#1533,.T.);
#1049=FACE_OUTER_BOUND('',#1539,.T.);
#1050=FACE_OUTER_BOUND('',#1540,.T.);
#1051=FACE_OUTER_BOUND('',#1541,.T.);
#1052=FACE_OUTER_BOUND('',#1542,.T.);
#1053=FACE_OUTER_BOUND('',#1543,.T.);
#1054=FACE_OUTER_BOUND('',#1544,.T.);
#1055=FACE_OUTER_BOUND('',#1545,.T.);
#1056=FACE_OUTER_BOUND('',#1546,.T.);
#1057=FACE_OUTER_BOUND('',#1548,.T.);
#1058=FACE_OUTER_BOUND('',#1549,.T.);
#1059=FACE_OUTER_BOUND('',#1551,.T.);
#1060=FACE_OUTER_BOUND('',#1552,.T.);
#1061=FACE_OUTER_BOUND('',#1553,.T.);
#1062=FACE_OUTER_BOUND('',#1554,.T.);
#1063=FACE_OUTER_BOUND('',#1556,.T.);
#1064=FACE_OUTER_BOUND('',#1557,.T.);
#1065=FACE_OUTER_BOUND('',#1558,.T.);
#1066=FACE_OUTER_BOUND('',#1559,.T.);
#1067=FACE_OUTER_BOUND('',#1561,.T.);
#1068=FACE_OUTER_BOUND('',#1562,.T.);
#1069=FACE_OUTER_BOUND('',#1563,.T.);
#1070=FACE_OUTER_BOUND('',#1564,.T.);
#1071=FACE_OUTER_BOUND('',#1565,.T.);
#1072=FACE_OUTER_BOUND('',#1566,.T.);
#1073=FACE_OUTER_BOUND('',#1567,.T.);
#1074=FACE_OUTER_BOUND('',#1568,.T.);
#1075=FACE_OUTER_BOUND('',#1569,.T.);
#1076=FACE_OUTER_BOUND('',#1570,.T.);
#1077=FACE_OUTER_BOUND('',#1571,.T.);
#1078=FACE_OUTER_BOUND('',#1572,.T.);
#1079=FACE_OUTER_BOUND('',#1573,.T.);
#1080=FACE_OUTER_BOUND('',#1574,.T.);
#1081=FACE_OUTER_BOUND('',#1575,.T.);
#1082=FACE_OUTER_BOUND('',#1576,.T.);
#1083=FACE_OUTER_BOUND('',#1577,.T.);
#1084=FACE_OUTER_BOUND('',#1578,.T.);
#1085=FACE_OUTER_BOUND('',#1579,.T.);
#1086=FACE_OUTER_BOUND('',#1580,.T.);
#1087=FACE_OUTER_BOUND('',#1581,.T.);
#1088=FACE_OUTER_BOUND('',#1582,.T.);
#1089=FACE_OUTER_BOUND('',#1583,.T.);
#1090=FACE_OUTER_BOUND('',#1584,.T.);
#1091=FACE_OUTER_BOUND('',#1586,.T.);
#1092=FACE_OUTER_BOUND('',#1587,.T.);
#1093=FACE_OUTER_BOUND('',#1589,.T.);
#1094=FACE_OUTER_BOUND('',#1590,.T.);
#1095=FACE_OUTER_BOUND('',#1592,.T.);
#1096=FACE_OUTER_BOUND('',#1593,.T.);
#1097=FACE_OUTER_BOUND('',#1595,.T.);
#1098=FACE_OUTER_BOUND('',#1596,.T.);
#1099=FACE_OUTER_BOUND('',#1598,.T.);
#1100=FACE_OUTER_BOUND('',#1599,.T.);
#1101=FACE_OUTER_BOUND('',#1600,.T.);
#1102=FACE_OUTER_BOUND('',#1601,.T.);
#1103=FACE_OUTER_BOUND('',#1602,.T.);
#1104=FACE_OUTER_BOUND('',#1603,.T.);
#1105=FACE_OUTER_BOUND('',#1605,.T.);
#1106=FACE_OUTER_BOUND('',#1606,.T.);
#1107=FACE_OUTER_BOUND('',#1607,.T.);
#1108=FACE_OUTER_BOUND('',#1608,.T.);
#1109=FACE_OUTER_BOUND('',#1609,.T.);
#1110=FACE_OUTER_BOUND('',#1610,.T.);
#1111=FACE_OUTER_BOUND('',#1611,.T.);
#1112=FACE_OUTER_BOUND('',#1612,.T.);
#1113=FACE_OUTER_BOUND('',#1613,.T.);
#1114=FACE_OUTER_BOUND('',#1614,.T.);
#1115=FACE_OUTER_BOUND('',#1615,.T.);
#1116=FACE_OUTER_BOUND('',#1616,.T.);
#1117=FACE_OUTER_BOUND('',#1617,.T.);
#1118=FACE_OUTER_BOUND('',#1618,.T.);
#1119=FACE_OUTER_BOUND('',#1619,.T.);
#1120=FACE_OUTER_BOUND('',#1620,.T.);
#1121=FACE_OUTER_BOUND('',#1621,.T.);
#1122=FACE_OUTER_BOUND('',#1622,.T.);
#1123=FACE_OUTER_BOUND('',#1624,.T.);
#1124=FACE_OUTER_BOUND('',#1625,.T.);
#1125=FACE_OUTER_BOUND('',#1627,.T.);
#1126=FACE_OUTER_BOUND('',#1628,.T.);
#1127=FACE_OUTER_BOUND('',#1630,.T.);
#1128=FACE_OUTER_BOUND('',#1631,.T.);
#1129=FACE_OUTER_BOUND('',#1633,.T.);
#1130=FACE_OUTER_BOUND('',#1634,.T.);
#1131=FACE_OUTER_BOUND('',#1636,.T.);
#1132=FACE_OUTER_BOUND('',#1637,.T.);
#1133=FACE_OUTER_BOUND('',#1639,.T.);
#1134=FACE_OUTER_BOUND('',#1641,.T.);
#1135=FACE_OUTER_BOUND('',#1642,.T.);
#1136=FACE_OUTER_BOUND('',#1643,.T.);
#1137=FACE_OUTER_BOUND('',#1644,.T.);
#1138=FACE_OUTER_BOUND('',#1645,.T.);
#1139=FACE_OUTER_BOUND('',#1647,.T.);
#1140=FACE_OUTER_BOUND('',#1649,.T.);
#1141=FACE_OUTER_BOUND('',#1651,.T.);
#1142=FACE_OUTER_BOUND('',#1653,.T.);
#1143=FACE_OUTER_BOUND('',#1654,.T.);
#1144=FACE_OUTER_BOUND('',#1655,.T.);
#1145=FACE_OUTER_BOUND('',#1656,.T.);
#1146=FACE_OUTER_BOUND('',#1657,.T.);
#1147=FACE_OUTER_BOUND('',#1658,.T.);
#1148=FACE_OUTER_BOUND('',#1659,.T.);
#1149=FACE_OUTER_BOUND('',#1660,.T.);
#1150=FACE_OUTER_BOUND('',#1661,.T.);
#1151=FACE_OUTER_BOUND('',#1662,.T.);
#1152=FACE_OUTER_BOUND('',#1663,.T.);
#1153=FACE_OUTER_BOUND('',#1664,.T.);
#1154=FACE_OUTER_BOUND('',#1665,.T.);
#1155=FACE_OUTER_BOUND('',#1666,.T.);
#1156=FACE_OUTER_BOUND('',#1668,.T.);
#1157=FACE_OUTER_BOUND('',#1669,.T.);
#1158=FACE_OUTER_BOUND('',#1670,.T.);
#1159=FACE_OUTER_BOUND('',#1671,.T.);
#1160=FACE_OUTER_BOUND('',#1672,.T.);
#1161=FACE_OUTER_BOUND('',#1673,.T.);
#1162=FACE_OUTER_BOUND('',#1674,.T.);
#1163=FACE_OUTER_BOUND('',#1675,.T.);
#1164=FACE_OUTER_BOUND('',#1676,.T.);
#1165=FACE_OUTER_BOUND('',#1677,.T.);
#1166=FACE_OUTER_BOUND('',#1678,.T.);
#1167=FACE_OUTER_BOUND('',#1679,.T.);
#1168=FACE_OUTER_BOUND('',#1680,.T.);
#1169=FACE_OUTER_BOUND('',#1681,.T.);
#1170=FACE_OUTER_BOUND('',#1682,.T.);
#1171=FACE_OUTER_BOUND('',#1683,.T.);
#1172=FACE_OUTER_BOUND('',#1684,.T.);
#1173=FACE_OUTER_BOUND('',#1687,.T.);
#1174=FACE_OUTER_BOUND('',#1689,.T.);
#1175=FACE_OUTER_BOUND('',#1691,.T.);
#1176=FACE_OUTER_BOUND('',#1692,.T.);
#1177=FACE_OUTER_BOUND('',#1693,.T.);
#1178=FACE_OUTER_BOUND('',#1695,.T.);
#1179=FACE_OUTER_BOUND('',#1697,.T.);
#1180=FACE_OUTER_BOUND('',#1698,.T.);
#1181=FACE_OUTER_BOUND('',#1699,.T.);
#1182=FACE_OUTER_BOUND('',#1701,.T.);
#1183=FACE_OUTER_BOUND('',#1703,.T.);
#1184=FACE_OUTER_BOUND('',#1704,.T.);
#1185=FACE_OUTER_BOUND('',#1705,.T.);
#1186=FACE_OUTER_BOUND('',#1707,.T.);
#1187=FACE_OUTER_BOUND('',#1709,.T.);
#1188=FACE_OUTER_BOUND('',#1710,.T.);
#1189=FACE_OUTER_BOUND('',#1711,.T.);
#1190=FACE_OUTER_BOUND('',#1713,.T.);
#1191=FACE_OUTER_BOUND('',#1715,.T.);
#1192=FACE_OUTER_BOUND('',#1716,.T.);
#1193=FACE_OUTER_BOUND('',#1717,.T.);
#1194=FACE_OUTER_BOUND('',#1718,.T.);
#1195=FACE_OUTER_BOUND('',#1720,.T.);
#1196=FACE_OUTER_BOUND('',#1721,.T.);
#1197=FACE_OUTER_BOUND('',#1722,.T.);
#1198=FACE_OUTER_BOUND('',#1723,.T.);
#1199=FACE_OUTER_BOUND('',#1725,.T.);
#1200=FACE_OUTER_BOUND('',#1726,.T.);
#1201=FACE_OUTER_BOUND('',#1728,.T.);
#1202=FACE_OUTER_BOUND('',#1730,.T.);
#1203=FACE_OUTER_BOUND('',#1731,.T.);
#1204=FACE_OUTER_BOUND('',#1732,.T.);
#1205=FACE_OUTER_BOUND('',#1733,.T.);
#1206=FACE_OUTER_BOUND('',#1734,.T.);
#1207=FACE_OUTER_BOUND('',#1736,.T.);
#1208=FACE_OUTER_BOUND('',#1737,.T.);
#1209=FACE_OUTER_BOUND('',#1738,.T.);
#1210=FACE_OUTER_BOUND('',#1740,.T.);
#1211=FACE_OUTER_BOUND('',#1741,.T.);
#1212=FACE_OUTER_BOUND('',#1742,.T.);
#1213=FACE_OUTER_BOUND('',#1744,.T.);
#1214=FACE_OUTER_BOUND('',#1746,.T.);
#1215=FACE_OUTER_BOUND('',#1748,.T.);
#1216=FACE_OUTER_BOUND('',#1749,.T.);
#1217=FACE_OUTER_BOUND('',#1750,.T.);
#1218=FACE_OUTER_BOUND('',#1751,.T.);
#1219=FACE_OUTER_BOUND('',#1752,.T.);
#1220=FACE_OUTER_BOUND('',#1754,.T.);
#1221=FACE_OUTER_BOUND('',#1755,.T.);
#1222=FACE_OUTER_BOUND('',#1756,.T.);
#1223=FACE_OUTER_BOUND('',#1758,.T.);
#1224=FACE_OUTER_BOUND('',#1760,.T.);
#1225=FACE_OUTER_BOUND('',#1761,.T.);
#1226=FACE_OUTER_BOUND('',#1762,.T.);
#1227=FACE_OUTER_BOUND('',#1764,.T.);
#1228=FACE_OUTER_BOUND('',#1766,.T.);
#1229=FACE_OUTER_BOUND('',#1767,.T.);
#1230=FACE_OUTER_BOUND('',#1768,.T.);
#1231=FACE_OUTER_BOUND('',#1769,.T.);
#1232=FACE_OUTER_BOUND('',#1770,.T.);
#1233=FACE_OUTER_BOUND('',#1771,.T.);
#1234=FACE_OUTER_BOUND('',#1772,.T.);
#1235=FACE_OUTER_BOUND('',#1773,.T.);
#1236=FACE_OUTER_BOUND('',#1774,.T.);
#1237=FACE_OUTER_BOUND('',#1775,.T.);
#1238=FACE_OUTER_BOUND('',#1776,.T.);
#1239=FACE_OUTER_BOUND('',#1777,.T.);
#1240=FACE_OUTER_BOUND('',#1778,.T.);
#1241=FACE_OUTER_BOUND('',#1779,.T.);
#1242=FACE_OUTER_BOUND('',#1780,.T.);
#1243=FACE_OUTER_BOUND('',#1782,.T.);
#1244=FACE_OUTER_BOUND('',#1783,.T.);
#1245=FACE_OUTER_BOUND('',#1784,.T.);
#1246=FACE_OUTER_BOUND('',#1785,.T.);
#1247=FACE_OUTER_BOUND('',#1786,.T.);
#1248=FACE_OUTER_BOUND('',#1787,.T.);
#1249=FACE_OUTER_BOUND('',#1788,.T.);
#1250=FACE_OUTER_BOUND('',#1789,.T.);
#1251=FACE_OUTER_BOUND('',#1790,.T.);
#1252=FACE_OUTER_BOUND('',#1791,.T.);
#1253=FACE_OUTER_BOUND('',#1792,.T.);
#1254=FACE_OUTER_BOUND('',#1793,.T.);
#1255=FACE_OUTER_BOUND('',#1794,.T.);
#1256=FACE_OUTER_BOUND('',#1795,.T.);
#1257=FACE_OUTER_BOUND('',#1796,.T.);
#1258=FACE_OUTER_BOUND('',#1797,.T.);
#1259=FACE_OUTER_BOUND('',#1798,.T.);
#1260=FACE_OUTER_BOUND('',#1799,.T.);
#1261=FACE_OUTER_BOUND('',#1801,.T.);
#1262=FACE_OUTER_BOUND('',#1803,.T.);
#1263=FACE_OUTER_BOUND('',#1804,.T.);
#1264=FACE_OUTER_BOUND('',#1805,.T.);
#1265=FACE_OUTER_BOUND('',#1806,.T.);
#1266=FACE_OUTER_BOUND('',#1807,.T.);
#1267=FACE_OUTER_BOUND('',#1813,.T.);
#1268=FACE_OUTER_BOUND('',#1814,.T.);
#1269=FACE_OUTER_BOUND('',#1815,.T.);
#1270=FACE_OUTER_BOUND('',#1816,.T.);
#1271=FACE_OUTER_BOUND('',#1817,.T.);
#1272=FACE_OUTER_BOUND('',#1822,.T.);
#1273=FACE_OUTER_BOUND('',#1823,.T.);
#1274=FACE_OUTER_BOUND('',#1824,.T.);
#1275=FACE_OUTER_BOUND('',#1825,.T.);
#1276=FACE_OUTER_BOUND('',#1827,.T.);
#1277=FACE_OUTER_BOUND('',#1828,.T.);
#1278=FACE_OUTER_BOUND('',#1829,.T.);
#1279=FACE_OUTER_BOUND('',#1831,.T.);
#1280=EDGE_LOOP('',(#4336,#4337,#4338,#4339));
#1281=EDGE_LOOP('',(#4340,#4341,#4342,#4343));
#1282=EDGE_LOOP('',(#4344,#4345,#4346,#4347));
#1283=EDGE_LOOP('',(#4348,#4349,#4350,#4351));
#1284=EDGE_LOOP('',(#4352,#4353,#4354,#4355));
#1285=EDGE_LOOP('',(#4356,#4357,#4358,#4359));
#1286=EDGE_LOOP('',(#4360,#4361,#4362,#4363));
#1287=EDGE_LOOP('',(#4364,#4365,#4366,#4367));
#1288=EDGE_LOOP('',(#4368,#4369,#4370,#4371));
#1289=EDGE_LOOP('',(#4372,#4373,#4374,#4375));
#1290=EDGE_LOOP('',(#4376,#4377,#4378,#4379));
#1291=EDGE_LOOP('',(#4380,#4381,#4382,#4383));
#1292=EDGE_LOOP('',(#4384,#4385,#4386,#4387));
#1293=EDGE_LOOP('',(#4388,#4389,#4390,#4391));
#1294=EDGE_LOOP('',(#4392,#4393,#4394,#4395));
#1295=EDGE_LOOP('',(#4396,#4397,#4398,#4399));
#1296=EDGE_LOOP('',(#4400));
#1297=EDGE_LOOP('',(#4401));
#1298=EDGE_LOOP('',(#4402));
#1299=EDGE_LOOP('',(#4403));
#1300=EDGE_LOOP('',(#4404));
#1301=EDGE_LOOP('',(#4405));
#1302=EDGE_LOOP('',(#4406,#4407,#4408,#4409));
#1303=EDGE_LOOP('',(#4410,#4411,#4412,#4413));
#1304=EDGE_LOOP('',(#4414));
#1305=EDGE_LOOP('',(#4415));
#1306=EDGE_LOOP('',(#4416));
#1307=EDGE_LOOP('',(#4417));
#1308=EDGE_LOOP('',(#4418));
#1309=EDGE_LOOP('',(#4419));
#1310=EDGE_LOOP('',(#4420,#4421,#4422,#4423));
#1311=EDGE_LOOP('',(#4424,#4425,#4426,#4427));
#1312=EDGE_LOOP('',(#4428,#4429,#4430,#4431));
#1313=EDGE_LOOP('',(#4432,#4433,#4434,#4435));
#1314=EDGE_LOOP('',(#4436,#4437,#4438,#4439));
#1315=EDGE_LOOP('',(#4440,#4441,#4442,#4443));
#1316=EDGE_LOOP('',(#4444,#4445,#4446,#4447));
#1317=EDGE_LOOP('',(#4448,#4449,#4450,#4451));
#1318=EDGE_LOOP('',(#4452,#4453,#4454,#4455));
#1319=EDGE_LOOP('',(#4456,#4457,#4458,#4459));
#1320=EDGE_LOOP('',(#4460,#4461,#4462,#4463));
#1321=EDGE_LOOP('',(#4464,#4465,#4466,#4467));
#1322=EDGE_LOOP('',(#4468,#4469,#4470,#4471));
#1323=EDGE_LOOP('',(#4472,#4473,#4474,#4475));
#1324=EDGE_LOOP('',(#4476,#4477,#4478,#4479));
#1325=EDGE_LOOP('',(#4480,#4481,#4482,#4483));
#1326=EDGE_LOOP('',(#4484,#4485,#4486,#4487));
#1327=EDGE_LOOP('',(#4488,#4489,#4490,#4491));
#1328=EDGE_LOOP('',(#4492,#4493,#4494,#4495));
#1329=EDGE_LOOP('',(#4496,#4497,#4498,#4499));
#1330=EDGE_LOOP('',(#4500));
#1331=EDGE_LOOP('',(#4501,#4502,#4503,#4504));
#1332=EDGE_LOOP('',(#4505));
#1333=EDGE_LOOP('',(#4506,#4507,#4508,#4509));
#1334=EDGE_LOOP('',(#4510,#4511,#4512,#4513));
#1335=EDGE_LOOP('',(#4514,#4515,#4516,#4517,#4518,#4519,#4520,#4521));
#1336=EDGE_LOOP('',(#4522));
#1337=EDGE_LOOP('',(#4523));
#1338=EDGE_LOOP('',(#4524));
#1339=EDGE_LOOP('',(#4525));
#1340=EDGE_LOOP('',(#4526));
#1341=EDGE_LOOP('',(#4527,#4528,#4529,#4530));
#1342=EDGE_LOOP('',(#4531,#4532,#4533,#4534,#4535,#4536,#4537,#4538));
#1343=EDGE_LOOP('',(#4539));
#1344=EDGE_LOOP('',(#4540));
#1345=EDGE_LOOP('',(#4541));
#1346=EDGE_LOOP('',(#4542));
#1347=EDGE_LOOP('',(#4543));
#1348=EDGE_LOOP('',(#4544,#4545,#4546,#4547));
#1349=EDGE_LOOP('',(#4548,#4549,#4550,#4551));
#1350=EDGE_LOOP('',(#4552,#4553,#4554,#4555));
#1351=EDGE_LOOP('',(#4556));
#1352=EDGE_LOOP('',(#4557));
#1353=EDGE_LOOP('',(#4558,#4559,#4560,#4561));
#1354=EDGE_LOOP('',(#4562,#4563,#4564,#4565));
#1355=EDGE_LOOP('',(#4566,#4567,#4568,#4569));
#1356=EDGE_LOOP('',(#4570,#4571,#4572,#4573));
#1357=EDGE_LOOP('',(#4574,#4575,#4576,#4577));
#1358=EDGE_LOOP('',(#4578));
#1359=EDGE_LOOP('',(#4579));
#1360=EDGE_LOOP('',(#4580,#4581,#4582,#4583));
#1361=EDGE_LOOP('',(#4584,#4585,#4586,#4587));
#1362=EDGE_LOOP('',(#4588));
#1363=EDGE_LOOP('',(#4589));
#1364=EDGE_LOOP('',(#4590));
#1365=EDGE_LOOP('',(#4591));
#1366=EDGE_LOOP('',(#4592));
#1367=EDGE_LOOP('',(#4593));
#1368=EDGE_LOOP('',(#4594));
#1369=EDGE_LOOP('',(#4595));
#1370=EDGE_LOOP('',(#4596));
#1371=EDGE_LOOP('',(#4597));
#1372=EDGE_LOOP('',(#4598));
#1373=EDGE_LOOP('',(#4599));
#1374=EDGE_LOOP('',(#4600,#4601,#4602,#4603));
#1375=EDGE_LOOP('',(#4604,#4605,#4606,#4607));
#1376=EDGE_LOOP('',(#4608,#4609,#4610,#4611));
#1377=EDGE_LOOP('',(#4612,#4613,#4614,#4615));
#1378=EDGE_LOOP('',(#4616,#4617,#4618,#4619));
#1379=EDGE_LOOP('',(#4620));
#1380=EDGE_LOOP('',(#4621));
#1381=EDGE_LOOP('',(#4622,#4623,#4624,#4625));
#1382=EDGE_LOOP('',(#4626,#4627,#4628,#4629));
#1383=EDGE_LOOP('',(#4630));
#1384=EDGE_LOOP('',(#4631));
#1385=EDGE_LOOP('',(#4632));
#1386=EDGE_LOOP('',(#4633));
#1387=EDGE_LOOP('',(#4634));
#1388=EDGE_LOOP('',(#4635));
#1389=EDGE_LOOP('',(#4636));
#1390=EDGE_LOOP('',(#4637));
#1391=EDGE_LOOP('',(#4638));
#1392=EDGE_LOOP('',(#4639));
#1393=EDGE_LOOP('',(#4640));
#1394=EDGE_LOOP('',(#4641));
#1395=EDGE_LOOP('',(#4642,#4643,#4644,#4645));
#1396=EDGE_LOOP('',(#4646,#4647,#4648,#4649));
#1397=EDGE_LOOP('',(#4650,#4651,#4652,#4653));
#1398=EDGE_LOOP('',(#4654,#4655,#4656,#4657));
#1399=EDGE_LOOP('',(#4658,#4659,#4660,#4661));
#1400=EDGE_LOOP('',(#4662,#4663,#4664,#4665));
#1401=EDGE_LOOP('',(#4666,#4667,#4668,#4669));
#1402=EDGE_LOOP('',(#4670,#4671,#4672,#4673));
#1403=EDGE_LOOP('',(#4674));
#1404=EDGE_LOOP('',(#4675,#4676,#4677,#4678));
#1405=EDGE_LOOP('',(#4679));
#1406=EDGE_LOOP('',(#4680,#4681,#4682,#4683));
#1407=EDGE_LOOP('',(#4684,#4685,#4686,#4687));
#1408=EDGE_LOOP('',(#4688,#4689,#4690,#4691,#4692,#4693,#4694,#4695));
#1409=EDGE_LOOP('',(#4696));
#1410=EDGE_LOOP('',(#4697));
#1411=EDGE_LOOP('',(#4698));
#1412=EDGE_LOOP('',(#4699));
#1413=EDGE_LOOP('',(#4700));
#1414=EDGE_LOOP('',(#4701,#4702,#4703,#4704));
#1415=EDGE_LOOP('',(#4705,#4706,#4707,#4708,#4709,#4710,#4711,#4712));
#1416=EDGE_LOOP('',(#4713));
#1417=EDGE_LOOP('',(#4714));
#1418=EDGE_LOOP('',(#4715));
#1419=EDGE_LOOP('',(#4716));
#1420=EDGE_LOOP('',(#4717));
#1421=EDGE_LOOP('',(#4718,#4719,#4720,#4721));
#1422=EDGE_LOOP('',(#4722,#4723,#4724,#4725));
#1423=EDGE_LOOP('',(#4726,#4727,#4728,#4729));
#1424=EDGE_LOOP('',(#4730));
#1425=EDGE_LOOP('',(#4731));
#1426=EDGE_LOOP('',(#4732,#4733,#4734,#4735));
#1427=EDGE_LOOP('',(#4736,#4737,#4738,#4739));
#1428=EDGE_LOOP('',(#4740,#4741,#4742,#4743));
#1429=EDGE_LOOP('',(#4744,#4745,#4746,#4747));
#1430=EDGE_LOOP('',(#4748,#4749,#4750,#4751));
#1431=EDGE_LOOP('',(#4752));
#1432=EDGE_LOOP('',(#4753));
#1433=EDGE_LOOP('',(#4754,#4755,#4756,#4757));
#1434=EDGE_LOOP('',(#4758,#4759,#4760,#4761));
#1435=EDGE_LOOP('',(#4762));
#1436=EDGE_LOOP('',(#4763));
#1437=EDGE_LOOP('',(#4764));
#1438=EDGE_LOOP('',(#4765));
#1439=EDGE_LOOP('',(#4766));
#1440=EDGE_LOOP('',(#4767));
#1441=EDGE_LOOP('',(#4768));
#1442=EDGE_LOOP('',(#4769));
#1443=EDGE_LOOP('',(#4770));
#1444=EDGE_LOOP('',(#4771));
#1445=EDGE_LOOP('',(#4772));
#1446=EDGE_LOOP('',(#4773));
#1447=EDGE_LOOP('',(#4774,#4775,#4776,#4777));
#1448=EDGE_LOOP('',(#4778,#4779,#4780,#4781));
#1449=EDGE_LOOP('',(#4782,#4783,#4784,#4785));
#1450=EDGE_LOOP('',(#4786,#4787,#4788,#4789));
#1451=EDGE_LOOP('',(#4790,#4791,#4792,#4793));
#1452=EDGE_LOOP('',(#4794));
#1453=EDGE_LOOP('',(#4795));
#1454=EDGE_LOOP('',(#4796,#4797,#4798,#4799));
#1455=EDGE_LOOP('',(#4800,#4801,#4802,#4803));
#1456=EDGE_LOOP('',(#4804));
#1457=EDGE_LOOP('',(#4805));
#1458=EDGE_LOOP('',(#4806));
#1459=EDGE_LOOP('',(#4807));
#1460=EDGE_LOOP('',(#4808));
#1461=EDGE_LOOP('',(#4809));
#1462=EDGE_LOOP('',(#4810));
#1463=EDGE_LOOP('',(#4811));
#1464=EDGE_LOOP('',(#4812));
#1465=EDGE_LOOP('',(#4813));
#1466=EDGE_LOOP('',(#4814));
#1467=EDGE_LOOP('',(#4815));
#1468=EDGE_LOOP('',(#4816,#4817,#4818,#4819));
#1469=EDGE_LOOP('',(#4820));
#1470=EDGE_LOOP('',(#4821,#4822,#4823,#4824));
#1471=EDGE_LOOP('',(#4825));
#1472=EDGE_LOOP('',(#4826,#4827,#4828,#4829));
#1473=EDGE_LOOP('',(#4830));
#1474=EDGE_LOOP('',(#4831,#4832,#4833,#4834));
#1475=EDGE_LOOP('',(#4835));
#1476=EDGE_LOOP('',(#4836,#4837,#4838,#4839));
#1477=EDGE_LOOP('',(#4840));
#1478=EDGE_LOOP('',(#4841));
#1479=EDGE_LOOP('',(#4842,#4843,#4844,#4845));
#1480=EDGE_LOOP('',(#4846,#4847,#4848,#4849));
#1481=EDGE_LOOP('',(#4850));
#1482=EDGE_LOOP('',(#4851));
#1483=EDGE_LOOP('',(#4852,#4853,#4854,#4855));
#1484=EDGE_LOOP('',(#4856,#4857,#4858,#4859));
#1485=EDGE_LOOP('',(#4860));
#1486=EDGE_LOOP('',(#4861));
#1487=EDGE_LOOP('',(#4862,#4863,#4864,#4865));
#1488=EDGE_LOOP('',(#4866,#4867,#4868,#4869,#4870,#4871,#4872,#4873,#4874,
#4875,#4876,#4877));
#1489=EDGE_LOOP('',(#4878));
#1490=EDGE_LOOP('',(#4879,#4880,#4881,#4882));
#1491=EDGE_LOOP('',(#4883,#4884,#4885,#4886));
#1492=EDGE_LOOP('',(#4887,#4888,#4889,#4890));
#1493=EDGE_LOOP('',(#4891,#4892,#4893,#4894));
#1494=EDGE_LOOP('',(#4895,#4896,#4897,#4898));
#1495=EDGE_LOOP('',(#4899));
#1496=EDGE_LOOP('',(#4900,#4901,#4902,#4903,#4904,#4905,#4906,#4907));
#1497=EDGE_LOOP('',(#4908,#4909,#4910,#4911));
#1498=EDGE_LOOP('',(#4912,#4913,#4914,#4915));
#1499=EDGE_LOOP('',(#4916,#4917,#4918,#4919));
#1500=EDGE_LOOP('',(#4920,#4921,#4922,#4923));
#1501=EDGE_LOOP('',(#4924,#4925,#4926,#4927,#4928,#4929,#4930,#4931));
#1502=EDGE_LOOP('',(#4932,#4933,#4934,#4935));
#1503=EDGE_LOOP('',(#4936));
#1504=EDGE_LOOP('',(#4937));
#1505=EDGE_LOOP('',(#4938));
#1506=EDGE_LOOP('',(#4939));
#1507=EDGE_LOOP('',(#4940));
#1508=EDGE_LOOP('',(#4941));
#1509=EDGE_LOOP('',(#4942));
#1510=EDGE_LOOP('',(#4943,#4944,#4945,#4946));
#1511=EDGE_LOOP('',(#4947));
#1512=EDGE_LOOP('',(#4948,#4949,#4950,#4951));
#1513=EDGE_LOOP('',(#4952,#4953,#4954,#4955));
#1514=EDGE_LOOP('',(#4956));
#1515=EDGE_LOOP('',(#4957));
#1516=EDGE_LOOP('',(#4958));
#1517=EDGE_LOOP('',(#4959));
#1518=EDGE_LOOP('',(#4960,#4961,#4962,#4963));
#1519=EDGE_LOOP('',(#4964,#4965,#4966,#4967));
#1520=EDGE_LOOP('',(#4968,#4969,#4970,#4971));
#1521=EDGE_LOOP('',(#4972,#4973,#4974,#4975));
#1522=EDGE_LOOP('',(#4976,#4977,#4978,#4979));
#1523=EDGE_LOOP('',(#4980));
#1524=EDGE_LOOP('',(#4981));
#1525=EDGE_LOOP('',(#4982,#4983,#4984,#4985));
#1526=EDGE_LOOP('',(#4986,#4987,#4988,#4989));
#1527=EDGE_LOOP('',(#4990));
#1528=EDGE_LOOP('',(#4991));
#1529=EDGE_LOOP('',(#4992));
#1530=EDGE_LOOP('',(#4993));
#1531=EDGE_LOOP('',(#4994));
#1532=EDGE_LOOP('',(#4995));
#1533=EDGE_LOOP('',(#4996));
#1534=EDGE_LOOP('',(#4997));
#1535=EDGE_LOOP('',(#4998));
#1536=EDGE_LOOP('',(#4999));
#1537=EDGE_LOOP('',(#5000));
#1538=EDGE_LOOP('',(#5001));
#1539=EDGE_LOOP('',(#5002,#5003,#5004,#5005));
#1540=EDGE_LOOP('',(#5006));
#1541=EDGE_LOOP('',(#5007));
#1542=EDGE_LOOP('',(#5008,#5009,#5010,#5011,#5012,#5013));
#1543=EDGE_LOOP('',(#5014,#5015,#5016,#5017,#5018));
#1544=EDGE_LOOP('',(#5019,#5020,#5021,#5022));
#1545=EDGE_LOOP('',(#5023,#5024,#5025,#5026));
#1546=EDGE_LOOP('',(#5027));
#1547=EDGE_LOOP('',(#5028));
#1548=EDGE_LOOP('',(#5029,#5030,#5031,#5032,#5033));
#1549=EDGE_LOOP('',(#5034));
#1550=EDGE_LOOP('',(#5035));
#1551=EDGE_LOOP('',(#5036,#5037,#5038,#5039));
#1552=EDGE_LOOP('',(#5040,#5041,#5042,#5043,#5044,#5045));
#1553=EDGE_LOOP('',(#5046,#5047,#5048,#5049,#5050));
#1554=EDGE_LOOP('',(#5051));
#1555=EDGE_LOOP('',(#5052));
#1556=EDGE_LOOP('',(#5053,#5054,#5055,#5056));
#1557=EDGE_LOOP('',(#5057,#5058,#5059,#5060));
#1558=EDGE_LOOP('',(#5061,#5062,#5063,#5064));
#1559=EDGE_LOOP('',(#5065));
#1560=EDGE_LOOP('',(#5066));
#1561=EDGE_LOOP('',(#5067,#5068,#5069,#5070,#5071));
#1562=EDGE_LOOP('',(#5072,#5073));
#1563=EDGE_LOOP('',(#5074,#5075));
#1564=EDGE_LOOP('',(#5076,#5077));
#1565=EDGE_LOOP('',(#5078,#5079));
#1566=EDGE_LOOP('',(#5080,#5081));
#1567=EDGE_LOOP('',(#5082,#5083));
#1568=EDGE_LOOP('',(#5084,#5085));
#1569=EDGE_LOOP('',(#5086,#5087,#5088,#5089));
#1570=EDGE_LOOP('',(#5090,#5091,#5092,#5093,#5094,#5095,#5096,#5097,#5098,
#5099,#5100,#5101,#5102,#5103,#5104,#5105,#5106,#5107));
#1571=EDGE_LOOP('',(#5108,#5109,#5110,#5111));
#1572=EDGE_LOOP('',(#5112,#5113,#5114,#5115));
#1573=EDGE_LOOP('',(#5116,#5117,#5118,#5119));
#1574=EDGE_LOOP('',(#5120,#5121,#5122,#5123));
#1575=EDGE_LOOP('',(#5124,#5125,#5126,#5127,#5128,#5129));
#1576=EDGE_LOOP('',(#5130,#5131,#5132,#5133));
#1577=EDGE_LOOP('',(#5134,#5135,#5136,#5137));
#1578=EDGE_LOOP('',(#5138,#5139,#5140,#5141));
#1579=EDGE_LOOP('',(#5142,#5143,#5144,#5145));
#1580=EDGE_LOOP('',(#5146,#5147,#5148,#5149));
#1581=EDGE_LOOP('',(#5150,#5151,#5152,#5153,#5154,#5155,#5156,#5157,#5158,
#5159,#5160,#5161,#5162,#5163,#5164,#5165,#5166,#5167));
#1582=EDGE_LOOP('',(#5168,#5169,#5170,#5171));
#1583=EDGE_LOOP('',(#5172,#5173,#5174,#5175));
#1584=EDGE_LOOP('',(#5176));
#1585=EDGE_LOOP('',(#5177));
#1586=EDGE_LOOP('',(#5178,#5179,#5180,#5181));
#1587=EDGE_LOOP('',(#5182));
#1588=EDGE_LOOP('',(#5183));
#1589=EDGE_LOOP('',(#5184,#5185,#5186,#5187));
#1590=EDGE_LOOP('',(#5188));
#1591=EDGE_LOOP('',(#5189));
#1592=EDGE_LOOP('',(#5190,#5191,#5192,#5193));
#1593=EDGE_LOOP('',(#5194));
#1594=EDGE_LOOP('',(#5195));
#1595=EDGE_LOOP('',(#5196,#5197,#5198,#5199));
#1596=EDGE_LOOP('',(#5200));
#1597=EDGE_LOOP('',(#5201));
#1598=EDGE_LOOP('',(#5202,#5203,#5204,#5205));
#1599=EDGE_LOOP('',(#5206));
#1600=EDGE_LOOP('',(#5207,#5208,#5209,#5210));
#1601=EDGE_LOOP('',(#5211,#5212,#5213,#5214));
#1602=EDGE_LOOP('',(#5215,#5216,#5217,#5218));
#1603=EDGE_LOOP('',(#5219));
#1604=EDGE_LOOP('',(#5220));
#1605=EDGE_LOOP('',(#5221,#5222,#5223,#5224));
#1606=EDGE_LOOP('',(#5225,#5226,#5227,#5228));
#1607=EDGE_LOOP('',(#5229,#5230,#5231,#5232));
#1608=EDGE_LOOP('',(#5233));
#1609=EDGE_LOOP('',(#5234,#5235,#5236,#5237));
#1610=EDGE_LOOP('',(#5238,#5239,#5240,#5241));
#1611=EDGE_LOOP('',(#5242,#5243,#5244,#5245));
#1612=EDGE_LOOP('',(#5246,#5247,#5248,#5249));
#1613=EDGE_LOOP('',(#5250,#5251,#5252,#5253));
#1614=EDGE_LOOP('',(#5254,#5255,#5256,#5257));
#1615=EDGE_LOOP('',(#5258,#5259,#5260,#5261,#5262,#5263));
#1616=EDGE_LOOP('',(#5264,#5265,#5266,#5267,#5268,#5269));
#1617=EDGE_LOOP('',(#5270,#5271,#5272,#5273));
#1618=EDGE_LOOP('',(#5274,#5275,#5276,#5277));
#1619=EDGE_LOOP('',(#5278,#5279,#5280,#5281));
#1620=EDGE_LOOP('',(#5282,#5283,#5284,#5285));
#1621=EDGE_LOOP('',(#5286,#5287,#5288,#5289));
#1622=EDGE_LOOP('',(#5290));
#1623=EDGE_LOOP('',(#5291));
#1624=EDGE_LOOP('',(#5292,#5293,#5294,#5295));
#1625=EDGE_LOOP('',(#5296));
#1626=EDGE_LOOP('',(#5297));
#1627=EDGE_LOOP('',(#5298,#5299,#5300,#5301));
#1628=EDGE_LOOP('',(#5302));
#1629=EDGE_LOOP('',(#5303));
#1630=EDGE_LOOP('',(#5304,#5305,#5306,#5307));
#1631=EDGE_LOOP('',(#5308));
#1632=EDGE_LOOP('',(#5309));
#1633=EDGE_LOOP('',(#5310,#5311,#5312,#5313));
#1634=EDGE_LOOP('',(#5314));
#1635=EDGE_LOOP('',(#5315));
#1636=EDGE_LOOP('',(#5316,#5317,#5318,#5319));
#1637=EDGE_LOOP('',(#5320));
#1638=EDGE_LOOP('',(#5321));
#1639=EDGE_LOOP('',(#5322,#5323,#5324,#5325));
#1640=EDGE_LOOP('',(#5326,#5327,#5328,#5329));
#1641=EDGE_LOOP('',(#5330,#5331,#5332,#5333));
#1642=EDGE_LOOP('',(#5334,#5335,#5336,#5337));
#1643=EDGE_LOOP('',(#5338,#5339,#5340,#5341));
#1644=EDGE_LOOP('',(#5342,#5343,#5344,#5345));
#1645=EDGE_LOOP('',(#5346));
#1646=EDGE_LOOP('',(#5347));
#1647=EDGE_LOOP('',(#5348,#5349,#5350,#5351));
#1648=EDGE_LOOP('',(#5352,#5353,#5354,#5355));
#1649=EDGE_LOOP('',(#5356));
#1650=EDGE_LOOP('',(#5357));
#1651=EDGE_LOOP('',(#5358,#5359,#5360,#5361));
#1652=EDGE_LOOP('',(#5362,#5363,#5364,#5365));
#1653=EDGE_LOOP('',(#5366,#5367,#5368,#5369));
#1654=EDGE_LOOP('',(#5370,#5371,#5372,#5373));
#1655=EDGE_LOOP('',(#5374,#5375,#5376,#5377));
#1656=EDGE_LOOP('',(#5378,#5379,#5380,#5381));
#1657=EDGE_LOOP('',(#5382,#5383,#5384,#5385));
#1658=EDGE_LOOP('',(#5386,#5387,#5388,#5389));
#1659=EDGE_LOOP('',(#5390,#5391,#5392,#5393,#5394,#5395));
#1660=EDGE_LOOP('',(#5396,#5397,#5398,#5399,#5400,#5401));
#1661=EDGE_LOOP('',(#5402));
#1662=EDGE_LOOP('',(#5403));
#1663=EDGE_LOOP('',(#5404,#5405,#5406,#5407));
#1664=EDGE_LOOP('',(#5408,#5409,#5410,#5411));
#1665=EDGE_LOOP('',(#5412,#5413,#5414,#5415));
#1666=EDGE_LOOP('',(#5416));
#1667=EDGE_LOOP('',(#5417));
#1668=EDGE_LOOP('',(#5418,#5419,#5420,#5421));
#1669=EDGE_LOOP('',(#5422,#5423,#5424,#5425));
#1670=EDGE_LOOP('',(#5426,#5427,#5428,#5429));
#1671=EDGE_LOOP('',(#5430));
#1672=EDGE_LOOP('',(#5431,#5432,#5433,#5434));
#1673=EDGE_LOOP('',(#5435));
#1674=EDGE_LOOP('',(#5436,#5437,#5438,#5439));
#1675=EDGE_LOOP('',(#5440,#5441,#5442,#5443));
#1676=EDGE_LOOP('',(#5444,#5445,#5446,#5447));
#1677=EDGE_LOOP('',(#5448,#5449,#5450,#5451));
#1678=EDGE_LOOP('',(#5452,#5453,#5454,#5455));
#1679=EDGE_LOOP('',(#5456,#5457,#5458,#5459));
#1680=EDGE_LOOP('',(#5460,#5461,#5462,#5463));
#1681=EDGE_LOOP('',(#5464,#5465,#5466,#5467));
#1682=EDGE_LOOP('',(#5468,#5469,#5470,#5471));
#1683=EDGE_LOOP('',(#5472,#5473,#5474,#5475));
#1684=EDGE_LOOP('',(#5476,#5477,#5478,#5479));
#1685=EDGE_LOOP('',(#5480,#5481,#5482,#5483));
#1686=EDGE_LOOP('',(#5484,#5485,#5486,#5487));
#1687=EDGE_LOOP('',(#5488));
#1688=EDGE_LOOP('',(#5489));
#1689=EDGE_LOOP('',(#5490));
#1690=EDGE_LOOP('',(#5491));
#1691=EDGE_LOOP('',(#5492,#5493,#5494,#5495));
#1692=EDGE_LOOP('',(#5496,#5497,#5498,#5499));
#1693=EDGE_LOOP('',(#5500));
#1694=EDGE_LOOP('',(#5501));
#1695=EDGE_LOOP('',(#5502));
#1696=EDGE_LOOP('',(#5503));
#1697=EDGE_LOOP('',(#5504,#5505,#5506,#5507));
#1698=EDGE_LOOP('',(#5508,#5509,#5510,#5511));
#1699=EDGE_LOOP('',(#5512));
#1700=EDGE_LOOP('',(#5513));
#1701=EDGE_LOOP('',(#5514));
#1702=EDGE_LOOP('',(#5515));
#1703=EDGE_LOOP('',(#5516,#5517,#5518,#5519));
#1704=EDGE_LOOP('',(#5520,#5521,#5522,#5523));
#1705=EDGE_LOOP('',(#5524));
#1706=EDGE_LOOP('',(#5525));
#1707=EDGE_LOOP('',(#5526));
#1708=EDGE_LOOP('',(#5527));
#1709=EDGE_LOOP('',(#5528,#5529,#5530,#5531));
#1710=EDGE_LOOP('',(#5532,#5533,#5534,#5535));
#1711=EDGE_LOOP('',(#5536));
#1712=EDGE_LOOP('',(#5537));
#1713=EDGE_LOOP('',(#5538));
#1714=EDGE_LOOP('',(#5539));
#1715=EDGE_LOOP('',(#5540,#5541,#5542,#5543));
#1716=EDGE_LOOP('',(#5544,#5545,#5546,#5547));
#1717=EDGE_LOOP('',(#5548,#5549,#5550,#5551));
#1718=EDGE_LOOP('',(#5552));
#1719=EDGE_LOOP('',(#5553,#5554,#5555,#5556));
#1720=EDGE_LOOP('',(#5557,#5558,#5559,#5560));
#1721=EDGE_LOOP('',(#5561,#5562,#5563,#5564));
#1722=EDGE_LOOP('',(#5565,#5566,#5567,#5568));
#1723=EDGE_LOOP('',(#5569));
#1724=EDGE_LOOP('',(#5570,#5571,#5572,#5573));
#1725=EDGE_LOOP('',(#5574,#5575,#5576,#5577));
#1726=EDGE_LOOP('',(#5578));
#1727=EDGE_LOOP('',(#5579));
#1728=EDGE_LOOP('',(#5580));
#1729=EDGE_LOOP('',(#5581));
#1730=EDGE_LOOP('',(#5582,#5583,#5584,#5585));
#1731=EDGE_LOOP('',(#5586,#5587,#5588,#5589));
#1732=EDGE_LOOP('',(#5590,#5591,#5592,#5593));
#1733=EDGE_LOOP('',(#5594,#5595,#5596,#5597));
#1734=EDGE_LOOP('',(#5598));
#1735=EDGE_LOOP('',(#5599,#5600,#5601,#5602));
#1736=EDGE_LOOP('',(#5603,#5604,#5605,#5606));
#1737=EDGE_LOOP('',(#5607,#5608,#5609,#5610));
#1738=EDGE_LOOP('',(#5611,#5612,#5613,#5614));
#1739=EDGE_LOOP('',(#5615));
#1740=EDGE_LOOP('',(#5616,#5617,#5618,#5619));
#1741=EDGE_LOOP('',(#5620,#5621,#5622,#5623));
#1742=EDGE_LOOP('',(#5624,#5625,#5626,#5627));
#1743=EDGE_LOOP('',(#5628));
#1744=EDGE_LOOP('',(#5629,#5630,#5631,#5632));
#1745=EDGE_LOOP('',(#5633,#5634,#5635,#5636));
#1746=EDGE_LOOP('',(#5637));
#1747=EDGE_LOOP('',(#5638,#5639,#5640,#5641));
#1748=EDGE_LOOP('',(#5642,#5643,#5644,#5645));
#1749=EDGE_LOOP('',(#5646));
#1750=EDGE_LOOP('',(#5647,#5648,#5649,#5650));
#1751=EDGE_LOOP('',(#5651));
#1752=EDGE_LOOP('',(#5652));
#1753=EDGE_LOOP('',(#5653));
#1754=EDGE_LOOP('',(#5654,#5655,#5656,#5657));
#1755=EDGE_LOOP('',(#5658,#5659,#5660,#5661));
#1756=EDGE_LOOP('',(#5662));
#1757=EDGE_LOOP('',(#5663));
#1758=EDGE_LOOP('',(#5664));
#1759=EDGE_LOOP('',(#5665));
#1760=EDGE_LOOP('',(#5666,#5667,#5668,#5669));
#1761=EDGE_LOOP('',(#5670,#5671,#5672,#5673));
#1762=EDGE_LOOP('',(#5674));
#1763=EDGE_LOOP('',(#5675));
#1764=EDGE_LOOP('',(#5676));
#1765=EDGE_LOOP('',(#5677));
#1766=EDGE_LOOP('',(#5678,#5679,#5680,#5681,#5682,#5683,#5684,#5685));
#1767=EDGE_LOOP('',(#5686,#5687,#5688,#5689));
#1768=EDGE_LOOP('',(#5690,#5691,#5692,#5693));
#1769=EDGE_LOOP('',(#5694,#5695,#5696,#5697));
#1770=EDGE_LOOP('',(#5698,#5699,#5700,#5701));
#1771=EDGE_LOOP('',(#5702,#5703,#5704,#5705,#5706,#5707,#5708,#5709));
#1772=EDGE_LOOP('',(#5710,#5711,#5712,#5713));
#1773=EDGE_LOOP('',(#5714,#5715,#5716,#5717));
#1774=EDGE_LOOP('',(#5718,#5719,#5720,#5721));
#1775=EDGE_LOOP('',(#5722,#5723,#5724,#5725));
#1776=EDGE_LOOP('',(#5726));
#1777=EDGE_LOOP('',(#5727,#5728,#5729,#5730));
#1778=EDGE_LOOP('',(#5731,#5732,#5733,#5734));
#1779=EDGE_LOOP('',(#5735,#5736,#5737,#5738));
#1780=EDGE_LOOP('',(#5739));
#1781=EDGE_LOOP('',(#5740));
#1782=EDGE_LOOP('',(#5741,#5742,#5743,#5744));
#1783=EDGE_LOOP('',(#5745,#5746,#5747,#5748));
#1784=EDGE_LOOP('',(#5749,#5750,#5751,#5752));
#1785=EDGE_LOOP('',(#5753));
#1786=EDGE_LOOP('',(#5754,#5755,#5756,#5757));
#1787=EDGE_LOOP('',(#5758,#5759,#5760,#5761));
#1788=EDGE_LOOP('',(#5762,#5763,#5764,#5765));
#1789=EDGE_LOOP('',(#5766,#5767,#5768,#5769));
#1790=EDGE_LOOP('',(#5770,#5771,#5772,#5773));
#1791=EDGE_LOOP('',(#5774,#5775,#5776,#5777));
#1792=EDGE_LOOP('',(#5778,#5779,#5780,#5781,#5782,#5783));
#1793=EDGE_LOOP('',(#5784,#5785,#5786,#5787,#5788,#5789));
#1794=EDGE_LOOP('',(#5790,#5791,#5792,#5793));
#1795=EDGE_LOOP('',(#5794,#5795,#5796,#5797));
#1796=EDGE_LOOP('',(#5798,#5799,#5800,#5801));
#1797=EDGE_LOOP('',(#5802,#5803,#5804,#5805));
#1798=EDGE_LOOP('',(#5806,#5807,#5808,#5809));
#1799=EDGE_LOOP('',(#5810,#5811,#5812,#5813));
#1800=EDGE_LOOP('',(#5814));
#1801=EDGE_LOOP('',(#5815,#5816,#5817,#5818));
#1802=EDGE_LOOP('',(#5819));
#1803=EDGE_LOOP('',(#5820,#5821,#5822,#5823));
#1804=EDGE_LOOP('',(#5824,#5825,#5826,#5827));
#1805=EDGE_LOOP('',(#5828,#5829,#5830,#5831));
#1806=EDGE_LOOP('',(#5832,#5833,#5834,#5835));
#1807=EDGE_LOOP('',(#5836,#5837,#5838,#5839));
#1808=EDGE_LOOP('',(#5840));
#1809=EDGE_LOOP('',(#5841));
#1810=EDGE_LOOP('',(#5842));
#1811=EDGE_LOOP('',(#5843));
#1812=EDGE_LOOP('',(#5844));
#1813=EDGE_LOOP('',(#5845,#5846,#5847,#5848));
#1814=EDGE_LOOP('',(#5849,#5850,#5851,#5852));
#1815=EDGE_LOOP('',(#5853,#5854,#5855,#5856));
#1816=EDGE_LOOP('',(#5857,#5858,#5859,#5860));
#1817=EDGE_LOOP('',(#5861,#5862,#5863,#5864));
#1818=EDGE_LOOP('',(#5865));
#1819=EDGE_LOOP('',(#5866));
#1820=EDGE_LOOP('',(#5867));
#1821=EDGE_LOOP('',(#5868));
#1822=EDGE_LOOP('',(#5869,#5870,#5871,#5872));
#1823=EDGE_LOOP('',(#5873));
#1824=EDGE_LOOP('',(#5874,#5875,#5876,#5877));
#1825=EDGE_LOOP('',(#5878));
#1826=EDGE_LOOP('',(#5879));
#1827=EDGE_LOOP('',(#5880,#5881,#5882,#5883));
#1828=EDGE_LOOP('',(#5884,#5885,#5886,#5887));
#1829=EDGE_LOOP('',(#5888));
#1830=EDGE_LOOP('',(#5889));
#1831=EDGE_LOOP('',(#5890));
#1832=EDGE_LOOP('',(#5891));
#1833=LINE('',#9747,#2272);
#1834=LINE('',#9753,#2273);
#1835=LINE('',#9759,#2274);
#1836=LINE('',#9765,#2275);
#1837=LINE('',#9771,#2276);
#1838=LINE('',#9777,#2277);
#1839=LINE('',#9782,#2278);
#1840=LINE('',#9784,#2279);
#1841=LINE('',#9786,#2280);
#1842=LINE('',#9787,#2281);
#1843=LINE('',#9790,#2282);
#1844=LINE('',#9792,#2283);
#1845=LINE('',#9793,#2284);
#1846=LINE('',#9796,#2285);
#1847=LINE('',#9798,#2286);
#1848=LINE('',#9799,#2287);
#1849=LINE('',#9801,#2288);
#1850=LINE('',#9802,#2289);
#1851=LINE('',#9807,#2290);
#1852=LINE('',#9809,#2291);
#1853=LINE('',#9811,#2292);
#1854=LINE('',#9812,#2293);
#1855=LINE('',#9815,#2294);
#1856=LINE('',#9817,#2295);
#1857=LINE('',#9818,#2296);
#1858=LINE('',#9821,#2297);
#1859=LINE('',#9823,#2298);
#1860=LINE('',#9824,#2299);
#1861=LINE('',#9826,#2300);
#1862=LINE('',#9827,#2301);
#1863=LINE('',#9834,#2302);
#1864=LINE('',#9836,#2303);
#1865=LINE('',#9838,#2304);
#1866=LINE('',#9839,#2305);
#1867=LINE('',#9842,#2306);
#1868=LINE('',#9844,#2307);
#1869=LINE('',#9845,#2308);
#1870=LINE('',#9848,#2309);
#1871=LINE('',#9850,#2310);
#1872=LINE('',#9851,#2311);
#1873=LINE('',#9853,#2312);
#1874=LINE('',#9854,#2313);
#1875=LINE('',#9861,#2314);
#1876=LINE('',#9863,#2315);
#1877=LINE('',#9865,#2316);
#1878=LINE('',#9866,#2317);
#1879=LINE('',#9869,#2318);
#1880=LINE('',#9871,#2319);
#1881=LINE('',#9872,#2320);
#1882=LINE('',#9875,#2321);
#1883=LINE('',#9877,#2322);
#1884=LINE('',#9878,#2323);
#1885=LINE('',#9880,#2324);
#1886=LINE('',#9881,#2325);
#1887=LINE('',#9889,#2326);
#1888=LINE('',#9895,#2327);
#1889=LINE('',#9901,#2328);
#1890=LINE('',#9907,#2329);
#1891=LINE('',#9913,#2330);
#1892=LINE('',#9919,#2331);
#1893=LINE('',#9925,#2332);
#1894=LINE('',#9930,#2333);
#1895=LINE('',#9932,#2334);
#1896=LINE('',#9934,#2335);
#1897=LINE('',#9935,#2336);
#1898=LINE('',#9939,#2337);
#1899=LINE('',#9941,#2338);
#1900=LINE('',#9943,#2339);
#1901=LINE('',#9944,#2340);
#1902=LINE('',#9947,#2341);
#1903=LINE('',#9949,#2342);
#1904=LINE('',#9950,#2343);
#1905=LINE('',#9953,#2344);
#1906=LINE('',#9955,#2345);
#1907=LINE('',#9956,#2346);
#1908=LINE('',#9959,#2347);
#1909=LINE('',#9961,#2348);
#1910=LINE('',#9962,#2349);
#1911=LINE('',#9963,#2350);
#1912=LINE('',#9966,#2351);
#1913=LINE('',#9967,#2352);
#1914=LINE('',#9970,#2353);
#1915=LINE('',#9971,#2354);
#1916=LINE('',#9972,#2355);
#1917=LINE('',#9974,#2356);
#1918=LINE('',#9982,#2357);
#1919=LINE('',#9988,#2358);
#1920=LINE('',#9994,#2359);
#1921=LINE('',#10000,#2360);
#1922=LINE('',#10006,#2361);
#1923=LINE('',#10013,#2362);
#1924=LINE('',#10019,#2363);
#1925=LINE('',#10028,#2364);
#1926=LINE('',#10034,#2365);
#1927=LINE('',#10040,#2366);
#1928=LINE('',#10046,#2367);
#1929=LINE('',#10052,#2368);
#1930=LINE('',#10060,#2369);
#1931=LINE('',#10065,#2370);
#1932=LINE('',#10074,#2371);
#1933=LINE('',#10080,#2372);
#1934=LINE('',#10086,#2373);
#1935=LINE('',#10092,#2374);
#1936=LINE('',#10098,#2375);
#1937=LINE('',#10104,#2376);
#1938=LINE('',#10110,#2377);
#1939=LINE('',#10115,#2378);
#1940=LINE('',#10117,#2379);
#1941=LINE('',#10119,#2380);
#1942=LINE('',#10120,#2381);
#1943=LINE('',#10124,#2382);
#1944=LINE('',#10126,#2383);
#1945=LINE('',#10128,#2384);
#1946=LINE('',#10129,#2385);
#1947=LINE('',#10132,#2386);
#1948=LINE('',#10134,#2387);
#1949=LINE('',#10135,#2388);
#1950=LINE('',#10138,#2389);
#1951=LINE('',#10140,#2390);
#1952=LINE('',#10141,#2391);
#1953=LINE('',#10144,#2392);
#1954=LINE('',#10146,#2393);
#1955=LINE('',#10147,#2394);
#1956=LINE('',#10148,#2395);
#1957=LINE('',#10151,#2396);
#1958=LINE('',#10152,#2397);
#1959=LINE('',#10155,#2398);
#1960=LINE('',#10156,#2399);
#1961=LINE('',#10157,#2400);
#1962=LINE('',#10159,#2401);
#1963=LINE('',#10167,#2402);
#1964=LINE('',#10173,#2403);
#1965=LINE('',#10179,#2404);
#1966=LINE('',#10185,#2405);
#1967=LINE('',#10191,#2406);
#1968=LINE('',#10198,#2407);
#1969=LINE('',#10204,#2408);
#1970=LINE('',#10213,#2409);
#1971=LINE('',#10219,#2410);
#1972=LINE('',#10225,#2411);
#1973=LINE('',#10231,#2412);
#1974=LINE('',#10237,#2413);
#1975=LINE('',#10245,#2414);
#1976=LINE('',#10250,#2415);
#1977=LINE('',#10259,#2416);
#1978=LINE('',#10266,#2417);
#1979=LINE('',#10273,#2418);
#1980=LINE('',#10280,#2419);
#1981=LINE('',#10287,#2420);
#1982=LINE('',#10295,#2421);
#1983=LINE('',#10300,#2422);
#1984=LINE('',#10308,#2423);
#1985=LINE('',#10313,#2424);
#1986=LINE('',#10321,#2425);
#1987=LINE('',#10325,#2426);
#1988=LINE('',#10327,#2427);
#1989=LINE('',#10329,#2428);
#1990=LINE('',#10331,#2429);
#1991=LINE('',#10333,#2430);
#1992=LINE('',#10335,#2431);
#1993=LINE('',#10337,#2432);
#1994=LINE('',#10339,#2433);
#1995=LINE('',#10341,#2434);
#1996=LINE('',#10343,#2435);
#1997=LINE('',#10345,#2436);
#1998=LINE('',#10346,#2437);
#1999=LINE('',#10350,#2438);
#2000=LINE('',#10351,#2439);
#2001=LINE('',#10352,#2440);
#2002=LINE('',#10356,#2441);
#2003=LINE('',#10357,#2442);
#2004=LINE('',#10358,#2443);
#2005=LINE('',#10361,#2444);
#2006=LINE('',#10363,#2445);
#2007=LINE('',#10364,#2446);
#2008=LINE('',#10367,#2447);
#2009=LINE('',#10368,#2448);
#2010=LINE('',#10371,#2449);
#2011=LINE('',#10372,#2450);
#2012=LINE('',#10374,#2451);
#2013=LINE('',#10375,#2452);
#2014=LINE('',#10379,#2453);
#2015=LINE('',#10381,#2454);
#2016=LINE('',#10382,#2455);
#2017=LINE('',#10385,#2456);
#2018=LINE('',#10386,#2457);
#2019=LINE('',#10389,#2458);
#2020=LINE('',#10390,#2459);
#2021=LINE('',#10392,#2460);
#2022=LINE('',#10393,#2461);
#2023=LINE('',#10401,#2462);
#2024=LINE('',#10407,#2463);
#2025=LINE('',#10416,#2464);
#2026=LINE('',#10422,#2465);
#2027=LINE('',#10428,#2466);
#2028=LINE('',#10434,#2467);
#2029=LINE('',#10440,#2468);
#2030=LINE('',#10448,#2469);
#2031=LINE('',#10453,#2470);
#2032=LINE('',#11842,#2471);
#2033=LINE('',#11848,#2472);
#2034=LINE('',#11852,#2473);
#2035=LINE('',#11858,#2474);
#2036=LINE('',#11863,#2475);
#2037=LINE('',#11878,#2476);
#2038=LINE('',#11887,#2477);
#2039=LINE('',#11891,#2478);
#2040=LINE('',#11895,#2479);
#2041=LINE('',#11898,#2480);
#2042=LINE('',#12034,#2481);
#2043=LINE('',#12287,#2482);
#2044=LINE('',#12329,#2483);
#2045=LINE('',#12334,#2484);
#2046=LINE('',#12343,#2485);
#2047=LINE('',#12348,#2486);
#2048=LINE('',#12361,#2487);
#2049=LINE('',#12365,#2488);
#2050=LINE('',#12369,#2489);
#2051=LINE('',#12376,#2490);
#2052=LINE('',#12380,#2491);
#2053=LINE('',#12384,#2492);
#2054=LINE('',#12389,#2493);
#2055=LINE('',#12391,#2494);
#2056=LINE('',#12393,#2495);
#2057=LINE('',#12394,#2496);
#2058=LINE('',#12397,#2497);
#2059=LINE('',#12399,#2498);
#2060=LINE('',#12400,#2499);
#2061=LINE('',#12403,#2500);
#2062=LINE('',#12405,#2501);
#2063=LINE('',#12406,#2502);
#2064=LINE('',#12409,#2503);
#2065=LINE('',#12411,#2504);
#2066=LINE('',#12412,#2505);
#2067=LINE('',#12415,#2506);
#2068=LINE('',#12417,#2507);
#2069=LINE('',#12418,#2508);
#2070=LINE('',#12420,#2509);
#2071=LINE('',#12421,#2510);
#2072=LINE('',#12431,#2511);
#2073=LINE('',#12433,#2512);
#2074=LINE('',#12434,#2513);
#2075=LINE('',#12437,#2514);
#2076=LINE('',#12439,#2515);
#2077=LINE('',#12440,#2516);
#2078=LINE('',#12445,#2517);
#2079=LINE('',#12446,#2518);
#2080=LINE('',#12448,#2519);
#2081=LINE('',#12449,#2520);
#2082=LINE('',#12459,#2521);
#2083=LINE('',#12466,#2522);
#2084=LINE('',#12473,#2523);
#2085=LINE('',#12480,#2524);
#2086=LINE('',#12487,#2525);
#2087=LINE('',#12492,#2526);
#2088=LINE('',#12499,#2527);
#2089=LINE('',#12502,#2528);
#2090=LINE('',#12505,#2529);
#2091=LINE('',#12507,#2530);
#2092=LINE('',#12508,#2531);
#2093=LINE('',#12514,#2532);
#2094=LINE('',#12516,#2533);
#2095=LINE('',#12517,#2534);
#2096=LINE('',#12526,#2535);
#2097=LINE('',#12531,#2536);
#2098=LINE('',#12538,#2537);
#2099=LINE('',#12540,#2538);
#2100=LINE('',#12542,#2539);
#2101=LINE('',#12543,#2540);
#2102=LINE('',#12546,#2541);
#2103=LINE('',#12548,#2542);
#2104=LINE('',#12549,#2543);
#2105=LINE('',#12552,#2544);
#2106=LINE('',#12554,#2545);
#2107=LINE('',#12555,#2546);
#2108=LINE('',#12558,#2547);
#2109=LINE('',#12560,#2548);
#2110=LINE('',#12561,#2549);
#2111=LINE('',#12564,#2550);
#2112=LINE('',#12566,#2551);
#2113=LINE('',#12567,#2552);
#2114=LINE('',#12569,#2553);
#2115=LINE('',#12570,#2554);
#2116=LINE('',#12582,#2555);
#2117=LINE('',#12586,#2556);
#2118=LINE('',#12590,#2557);
#2119=LINE('',#12597,#2558);
#2120=LINE('',#12599,#2559);
#2121=LINE('',#12606,#2560);
#2122=LINE('',#12613,#2561);
#2123=LINE('',#12619,#2562);
#2124=LINE('',#12621,#2563);
#2125=LINE('',#12623,#2564);
#2126=LINE('',#12624,#2565);
#2127=LINE('',#12629,#2566);
#2128=LINE('',#12630,#2567);
#2129=LINE('',#12633,#2568);
#2130=LINE('',#12635,#2569);
#2131=LINE('',#12636,#2570);
#2132=LINE('',#12638,#2571);
#2133=LINE('',#12644,#2572);
#2134=LINE('',#12646,#2573);
#2135=LINE('',#12648,#2574);
#2136=LINE('',#12649,#2575);
#2137=LINE('',#12654,#2576);
#2138=LINE('',#12655,#2577);
#2139=LINE('',#12658,#2578);
#2140=LINE('',#12660,#2579);
#2141=LINE('',#12661,#2580);
#2142=LINE('',#12663,#2581);
#2143=LINE('',#12670,#2582);
#2144=LINE('',#12679,#2583);
#2145=LINE('',#12685,#2584);
#2146=LINE('',#12694,#2585);
#2147=LINE('',#12700,#2586);
#2148=LINE('',#12709,#2587);
#2149=LINE('',#12715,#2588);
#2150=LINE('',#12724,#2589);
#2151=LINE('',#12730,#2590);
#2152=LINE('',#12738,#2591);
#2153=LINE('',#12740,#2592);
#2154=LINE('',#12742,#2593);
#2155=LINE('',#12743,#2594);
#2156=LINE('',#12746,#2595);
#2157=LINE('',#12748,#2596);
#2158=LINE('',#12749,#2597);
#2159=LINE('',#12752,#2598);
#2160=LINE('',#12754,#2599);
#2161=LINE('',#12755,#2600);
#2162=LINE('',#12766,#2601);
#2163=LINE('',#12770,#2602);
#2164=LINE('',#12777,#2603);
#2165=LINE('',#12786,#2604);
#2166=LINE('',#12791,#2605);
#2167=LINE('',#12793,#2606);
#2168=LINE('',#12795,#2607);
#2169=LINE('',#12796,#2608);
#2170=LINE('',#12799,#2609);
#2171=LINE('',#12801,#2610);
#2172=LINE('',#12802,#2611);
#2173=LINE('',#12805,#2612);
#2174=LINE('',#12807,#2613);
#2175=LINE('',#12808,#2614);
#2176=LINE('',#12818,#2615);
#2177=LINE('',#12822,#2616);
#2178=LINE('',#12826,#2617);
#2179=LINE('',#12829,#2618);
#2180=LINE('',#12832,#2619);
#2181=LINE('',#12833,#2620);
#2182=LINE('',#12836,#2621);
#2183=LINE('',#12837,#2622);
#2184=LINE('',#12842,#2623);
#2185=LINE('',#12850,#2624);
#2186=LINE('',#12857,#2625);
#2187=LINE('',#12866,#2626);
#2188=LINE('',#12872,#2627);
#2189=LINE('',#12881,#2628);
#2190=LINE('',#12887,#2629);
#2191=LINE('',#12895,#2630);
#2192=LINE('',#12897,#2631);
#2193=LINE('',#12899,#2632);
#2194=LINE('',#12901,#2633);
#2195=LINE('',#12903,#2634);
#2196=LINE('',#12905,#2635);
#2197=LINE('',#12907,#2636);
#2198=LINE('',#12908,#2637);
#2199=LINE('',#12911,#2638);
#2200=LINE('',#12913,#2639);
#2201=LINE('',#12914,#2640);
#2202=LINE('',#12917,#2641);
#2203=LINE('',#12918,#2642);
#2204=LINE('',#12921,#2643);
#2205=LINE('',#12922,#2644);
#2206=LINE('',#12925,#2645);
#2207=LINE('',#12926,#2646);
#2208=LINE('',#12929,#2647);
#2209=LINE('',#12931,#2648);
#2210=LINE('',#12933,#2649);
#2211=LINE('',#12934,#2650);
#2212=LINE('',#12936,#2651);
#2213=LINE('',#12938,#2652);
#2214=LINE('',#12940,#2653);
#2215=LINE('',#12949,#2654);
#2216=LINE('',#12953,#2655);
#2217=LINE('',#12957,#2656);
#2218=LINE('',#12964,#2657);
#2219=LINE('',#12968,#2658);
#2220=LINE('',#12972,#2659);
#2221=LINE('',#12977,#2660);
#2222=LINE('',#12979,#2661);
#2223=LINE('',#12981,#2662);
#2224=LINE('',#12982,#2663);
#2225=LINE('',#12985,#2664);
#2226=LINE('',#12987,#2665);
#2227=LINE('',#12988,#2666);
#2228=LINE('',#12991,#2667);
#2229=LINE('',#12993,#2668);
#2230=LINE('',#12994,#2669);
#2231=LINE('',#12997,#2670);
#2232=LINE('',#12999,#2671);
#2233=LINE('',#13000,#2672);
#2234=LINE('',#13003,#2673);
#2235=LINE('',#13005,#2674);
#2236=LINE('',#13006,#2675);
#2237=LINE('',#13008,#2676);
#2238=LINE('',#13009,#2677);
#2239=LINE('',#13076,#2678);
#2240=LINE('',#13081,#2679);
#2241=LINE('',#13083,#2680);
#2242=LINE('',#13085,#2681);
#2243=LINE('',#13086,#2682);
#2244=LINE('',#13089,#2683);
#2245=LINE('',#13091,#2684);
#2246=LINE('',#13092,#2685);
#2247=LINE('',#13095,#2686);
#2248=LINE('',#13097,#2687);
#2249=LINE('',#13098,#2688);
#2250=LINE('',#13100,#2689);
#2251=LINE('',#13101,#2690);
#2252=LINE('',#13109,#2691);
#2253=LINE('',#13115,#2692);
#2254=LINE('',#13121,#2693);
#2255=LINE('',#13127,#2694);
#2256=LINE('',#13132,#2695);
#2257=LINE('',#13134,#2696);
#2258=LINE('',#13136,#2697);
#2259=LINE('',#13137,#2698);
#2260=LINE('',#13142,#2699);
#2261=LINE('',#13144,#2700);
#2262=LINE('',#13145,#2701);
#2263=LINE('',#13148,#2702);
#2264=LINE('',#13149,#2703);
#2265=LINE('',#13152,#2704);
#2266=LINE('',#13153,#2705);
#2267=LINE('',#13155,#2706);
#2268=LINE('',#13161,#2707);
#2269=LINE('',#13166,#2708);
#2270=LINE('',#13174,#2709);
#2271=LINE('',#13180,#2710);
#2272=VECTOR('',#7679,0.21);
#2273=VECTOR('',#7686,0.21);
#2274=VECTOR('',#7693,0.165);
#2275=VECTOR('',#7700,0.165);
#2276=VECTOR('',#7707,0.165);
#2277=VECTOR('',#7714,0.165);
#2278=VECTOR('',#7719,1.);
#2279=VECTOR('',#7720,1.);
#2280=VECTOR('',#7721,1.);
#2281=VECTOR('',#7722,1.);
#2282=VECTOR('',#7725,1.);
#2283=VECTOR('',#7726,1.);
#2284=VECTOR('',#7727,1.);
#2285=VECTOR('',#7730,1.);
#2286=VECTOR('',#7731,1.);
#2287=VECTOR('',#7732,1.);
#2288=VECTOR('',#7735,1.);
#2289=VECTOR('',#7736,1.);
#2290=VECTOR('',#7741,1.);
#2291=VECTOR('',#7742,1.);
#2292=VECTOR('',#7743,1.);
#2293=VECTOR('',#7744,1.);
#2294=VECTOR('',#7747,1.);
#2295=VECTOR('',#7748,1.);
#2296=VECTOR('',#7749,1.);
#2297=VECTOR('',#7752,1.);
#2298=VECTOR('',#7753,1.);
#2299=VECTOR('',#7754,1.);
#2300=VECTOR('',#7757,1.);
#2301=VECTOR('',#7758,1.);
#2302=VECTOR('',#7767,1.);
#2303=VECTOR('',#7768,1.);
#2304=VECTOR('',#7769,1.);
#2305=VECTOR('',#7770,1.);
#2306=VECTOR('',#7773,1.);
#2307=VECTOR('',#7774,1.);
#2308=VECTOR('',#7775,1.);
#2309=VECTOR('',#7778,1.);
#2310=VECTOR('',#7779,1.);
#2311=VECTOR('',#7780,1.);
#2312=VECTOR('',#7783,1.);
#2313=VECTOR('',#7784,1.);
#2314=VECTOR('',#7793,1.);
#2315=VECTOR('',#7794,1.);
#2316=VECTOR('',#7795,1.);
#2317=VECTOR('',#7796,1.);
#2318=VECTOR('',#7799,1.);
#2319=VECTOR('',#7800,1.);
#2320=VECTOR('',#7801,1.);
#2321=VECTOR('',#7804,1.);
#2322=VECTOR('',#7805,1.);
#2323=VECTOR('',#7806,1.);
#2324=VECTOR('',#7809,1.);
#2325=VECTOR('',#7810,1.);
#2326=VECTOR('',#7821,0.225);
#2327=VECTOR('',#7828,0.225);
#2328=VECTOR('',#7835,0.165);
#2329=VECTOR('',#7842,0.165);
#2330=VECTOR('',#7849,0.165);
#2331=VECTOR('',#7856,0.165);
#2332=VECTOR('',#7863,1.6);
#2333=VECTOR('',#7868,1.);
#2334=VECTOR('',#7869,1.);
#2335=VECTOR('',#7870,1.);
#2336=VECTOR('',#7871,1.);
#2337=VECTOR('',#7874,1.);
#2338=VECTOR('',#7875,1.);
#2339=VECTOR('',#7876,1.);
#2340=VECTOR('',#7877,1.);
#2341=VECTOR('',#7880,1.);
#2342=VECTOR('',#7881,1.);
#2343=VECTOR('',#7882,1.);
#2344=VECTOR('',#7885,1.);
#2345=VECTOR('',#7886,1.);
#2346=VECTOR('',#7887,1.);
#2347=VECTOR('',#7890,1.);
#2348=VECTOR('',#7891,1.);
#2349=VECTOR('',#7892,1.);
#2350=VECTOR('',#7893,1.);
#2351=VECTOR('',#7896,1.);
#2352=VECTOR('',#7897,1.);
#2353=VECTOR('',#7900,1.);
#2354=VECTOR('',#7901,1.);
#2355=VECTOR('',#7902,1.);
#2356=VECTOR('',#7905,1.);
#2357=VECTOR('',#7916,0.225);
#2358=VECTOR('',#7923,0.225);
#2359=VECTOR('',#7930,0.225);
#2360=VECTOR('',#7937,0.225);
#2361=VECTOR('',#7944,1.59);
#2362=VECTOR('',#7953,1.005);
#2363=VECTOR('',#7960,2.4);
#2364=VECTOR('',#7973,0.225);
#2365=VECTOR('',#7980,0.225);
#2366=VECTOR('',#7987,0.225);
#2367=VECTOR('',#7994,0.225);
#2368=VECTOR('',#8001,1.59);
#2369=VECTOR('',#8012,1.005);
#2370=VECTOR('',#8017,2.4);
#2371=VECTOR('',#8030,0.225);
#2372=VECTOR('',#8037,0.225);
#2373=VECTOR('',#8044,0.165);
#2374=VECTOR('',#8051,0.165);
#2375=VECTOR('',#8058,0.165);
#2376=VECTOR('',#8065,0.165);
#2377=VECTOR('',#8072,1.6);
#2378=VECTOR('',#8077,1.);
#2379=VECTOR('',#8078,1.);
#2380=VECTOR('',#8079,1.);
#2381=VECTOR('',#8080,1.);
#2382=VECTOR('',#8083,1.);
#2383=VECTOR('',#8084,1.);
#2384=VECTOR('',#8085,1.);
#2385=VECTOR('',#8086,1.);
#2386=VECTOR('',#8089,1.);
#2387=VECTOR('',#8090,1.);
#2388=VECTOR('',#8091,1.);
#2389=VECTOR('',#8094,1.);
#2390=VECTOR('',#8095,1.);
#2391=VECTOR('',#8096,1.);
#2392=VECTOR('',#8099,1.);
#2393=VECTOR('',#8100,1.);
#2394=VECTOR('',#8101,1.);
#2395=VECTOR('',#8102,1.);
#2396=VECTOR('',#8105,1.);
#2397=VECTOR('',#8106,1.);
#2398=VECTOR('',#8109,1.);
#2399=VECTOR('',#8110,1.);
#2400=VECTOR('',#8111,1.);
#2401=VECTOR('',#8114,1.);
#2402=VECTOR('',#8125,0.225);
#2403=VECTOR('',#8132,0.225);
#2404=VECTOR('',#8139,0.225);
#2405=VECTOR('',#8146,0.225);
#2406=VECTOR('',#8153,1.59);
#2407=VECTOR('',#8162,1.005);
#2408=VECTOR('',#8169,2.4);
#2409=VECTOR('',#8182,0.225);
#2410=VECTOR('',#8189,0.225);
#2411=VECTOR('',#8196,0.225);
#2412=VECTOR('',#8203,0.225);
#2413=VECTOR('',#8210,1.59);
#2414=VECTOR('',#8221,1.005);
#2415=VECTOR('',#8226,2.4);
#2416=VECTOR('',#8239,0.165);
#2417=VECTOR('',#8248,0.165);
#2418=VECTOR('',#8257,0.165);
#2419=VECTOR('',#8266,0.165);
#2420=VECTOR('',#8275,1.05);
#2421=VECTOR('',#8286,0.625);
#2422=VECTOR('',#8291,0.5);
#2423=VECTOR('',#8302,0.275);
#2424=VECTOR('',#8307,0.5);
#2425=VECTOR('',#8318,0.275);
#2426=VECTOR('',#8321,1.);
#2427=VECTOR('',#8322,1.);
#2428=VECTOR('',#8323,1.);
#2429=VECTOR('',#8324,1.);
#2430=VECTOR('',#8325,1.);
#2431=VECTOR('',#8326,1.);
#2432=VECTOR('',#8327,1.);
#2433=VECTOR('',#8328,1.);
#2434=VECTOR('',#8329,1.);
#2435=VECTOR('',#8330,1.);
#2436=VECTOR('',#8331,1.);
#2437=VECTOR('',#8332,1.);
#2438=VECTOR('',#8335,1.);
#2439=VECTOR('',#8336,1.);
#2440=VECTOR('',#8337,1.);
#2441=VECTOR('',#8340,1.);
#2442=VECTOR('',#8341,1.);
#2443=VECTOR('',#8342,1.);
#2444=VECTOR('',#8345,1.);
#2445=VECTOR('',#8346,1.);
#2446=VECTOR('',#8347,1.);
#2447=VECTOR('',#8350,1.);
#2448=VECTOR('',#8351,1.);
#2449=VECTOR('',#8354,1.);
#2450=VECTOR('',#8355,1.);
#2451=VECTOR('',#8358,1.);
#2452=VECTOR('',#8359,1.);
#2453=VECTOR('',#8364,1.);
#2454=VECTOR('',#8365,1.);
#2455=VECTOR('',#8366,1.);
#2456=VECTOR('',#8369,1.);
#2457=VECTOR('',#8370,1.);
#2458=VECTOR('',#8373,1.);
#2459=VECTOR('',#8374,1.);
#2460=VECTOR('',#8377,1.);
#2461=VECTOR('',#8378,1.);
#2462=VECTOR('',#8389,0.625);
#2463=VECTOR('',#8396,1.04);
#2464=VECTOR('',#8409,0.225);
#2465=VECTOR('',#8416,0.225);
#2466=VECTOR('',#8423,0.225);
#2467=VECTOR('',#8430,0.225);
#2468=VECTOR('',#8437,1.04);
#2469=VECTOR('',#8448,0.625);
#2470=VECTOR('',#8453,1.8);
#2471=VECTOR('',#8488,1.070235);
#2472=VECTOR('',#8495,0.6);
#2473=VECTOR('',#8500,0.63);
#2474=VECTOR('',#8509,1.070235);
#2475=VECTOR('',#8516,0.63);
#2476=VECTOR('',#8535,1.129765);
#2477=VECTOR('',#8546,1.57);
#2478=VECTOR('',#8551,1.6);
#2479=VECTOR('',#8556,1.57);
#2480=VECTOR('',#8561,1.129765);
#2481=VECTOR('',#8608,1.123812);
#2482=VECTOR('',#8677,1.076188);
#2483=VECTOR('',#8706,1.119765);
#2484=VECTOR('',#8713,1.085235);
#2485=VECTOR('',#8724,1.119765);
#2486=VECTOR('',#8731,1.085235);
#2487=VECTOR('',#8752,0.4);
#2488=VECTOR('',#8757,0.425);
#2489=VECTOR('',#8762,0.41);
#2490=VECTOR('',#8771,0.26);
#2491=VECTOR('',#8776,0.25);
#2492=VECTOR('',#8781,0.225);
#2493=VECTOR('',#8786,1.);
#2494=VECTOR('',#8787,1.);
#2495=VECTOR('',#8788,1.);
#2496=VECTOR('',#8789,1.);
#2497=VECTOR('',#8792,1.);
#2498=VECTOR('',#8793,1.);
#2499=VECTOR('',#8794,1.);
#2500=VECTOR('',#8797,1.);
#2501=VECTOR('',#8798,1.);
#2502=VECTOR('',#8799,1.);
#2503=VECTOR('',#8802,1.);
#2504=VECTOR('',#8803,1.);
#2505=VECTOR('',#8804,1.);
#2506=VECTOR('',#8807,1.);
#2507=VECTOR('',#8808,1.);
#2508=VECTOR('',#8809,1.);
#2509=VECTOR('',#8812,1.);
#2510=VECTOR('',#8813,1.);
#2511=VECTOR('',#8826,1.);
#2512=VECTOR('',#8827,1.);
#2513=VECTOR('',#8828,1.);
#2514=VECTOR('',#8831,1.);
#2515=VECTOR('',#8832,1.);
#2516=VECTOR('',#8833,1.);
#2517=VECTOR('',#8838,1.);
#2518=VECTOR('',#8839,1.);
#2519=VECTOR('',#8842,1.);
#2520=VECTOR('',#8843,1.);
#2521=VECTOR('',#8856,1.05);
#2522=VECTOR('',#8865,1.);
#2523=VECTOR('',#8874,1.05);
#2524=VECTOR('',#8883,1.);
#2525=VECTOR('',#8892,1.05);
#2526=VECTOR('',#8899,0.9);
#2527=VECTOR('',#8906,1.);
#2528=VECTOR('',#8909,1.);
#2529=VECTOR('',#8912,1.);
#2530=VECTOR('',#8913,1.);
#2531=VECTOR('',#8914,1.);
#2532=VECTOR('',#8921,1.);
#2533=VECTOR('',#8924,1.);
#2534=VECTOR('',#8925,1.);
#2535=VECTOR('',#8936,0.895);
#2536=VECTOR('',#8943,0.605);
#2537=VECTOR('',#8952,1.);
#2538=VECTOR('',#8953,1.);
#2539=VECTOR('',#8954,1.);
#2540=VECTOR('',#8955,1.);
#2541=VECTOR('',#8958,1.);
#2542=VECTOR('',#8959,1.);
#2543=VECTOR('',#8960,1.);
#2544=VECTOR('',#8963,1.);
#2545=VECTOR('',#8964,1.);
#2546=VECTOR('',#8965,1.);
#2547=VECTOR('',#8968,1.);
#2548=VECTOR('',#8969,1.);
#2549=VECTOR('',#8970,1.);
#2550=VECTOR('',#8973,1.);
#2551=VECTOR('',#8974,1.);
#2552=VECTOR('',#8975,1.);
#2553=VECTOR('',#8978,1.);
#2554=VECTOR('',#8979,1.);
#2555=VECTOR('',#8996,0.325);
#2556=VECTOR('',#9001,0.35);
#2557=VECTOR('',#9006,0.335);
#2558=VECTOR('',#9015,0.21);
#2559=VECTOR('',#9018,0.2);
#2560=VECTOR('',#9027,0.165);
#2561=VECTOR('',#9036,0.165);
#2562=VECTOR('',#9043,1.);
#2563=VECTOR('',#9044,1.);
#2564=VECTOR('',#9045,1.);
#2565=VECTOR('',#9046,1.);
#2566=VECTOR('',#9051,1.);
#2567=VECTOR('',#9052,1.);
#2568=VECTOR('',#9055,1.);
#2569=VECTOR('',#9056,1.);
#2570=VECTOR('',#9057,1.);
#2571=VECTOR('',#9060,1.);
#2572=VECTOR('',#9067,1.);
#2573=VECTOR('',#9068,1.);
#2574=VECTOR('',#9069,1.);
#2575=VECTOR('',#9070,1.);
#2576=VECTOR('',#9075,1.);
#2577=VECTOR('',#9076,1.);
#2578=VECTOR('',#9079,1.);
#2579=VECTOR('',#9080,1.);
#2580=VECTOR('',#9081,1.);
#2581=VECTOR('',#9084,1.);
#2582=VECTOR('',#9093,0.6);
#2583=VECTOR('',#9106,0.605);
#2584=VECTOR('',#9113,0.8);
#2585=VECTOR('',#9126,0.605);
#2586=VECTOR('',#9133,0.8);
#2587=VECTOR('',#9146,0.605);
#2588=VECTOR('',#9153,0.8);
#2589=VECTOR('',#9166,0.605);
#2590=VECTOR('',#9173,0.8);
#2591=VECTOR('',#9184,1.);
#2592=VECTOR('',#9185,1.);
#2593=VECTOR('',#9186,1.);
#2594=VECTOR('',#9187,1.);
#2595=VECTOR('',#9190,1.);
#2596=VECTOR('',#9191,1.);
#2597=VECTOR('',#9192,1.);
#2598=VECTOR('',#9195,1.);
#2599=VECTOR('',#9196,1.);
#2600=VECTOR('',#9197,1.);
#2601=VECTOR('',#9212,0.9);
#2602=VECTOR('',#9217,0.9);
#2603=VECTOR('',#9226,2.);
#2604=VECTOR('',#9239,0.225);
#2605=VECTOR('',#9244,1.);
#2606=VECTOR('',#9245,1.);
#2607=VECTOR('',#9246,1.);
#2608=VECTOR('',#9247,1.);
#2609=VECTOR('',#9250,1.);
#2610=VECTOR('',#9251,1.);
#2611=VECTOR('',#9252,1.);
#2612=VECTOR('',#9255,1.);
#2613=VECTOR('',#9256,1.);
#2614=VECTOR('',#9257,1.);
#2615=VECTOR('',#9270,1.);
#2616=VECTOR('',#9273,1.);
#2617=VECTOR('',#9278,1.);
#2618=VECTOR('',#9281,1.);
#2619=VECTOR('',#9284,1.);
#2620=VECTOR('',#9285,1.);
#2621=VECTOR('',#9288,1.);
#2622=VECTOR('',#9289,1.);
#2623=VECTOR('',#9296,1.2);
#2624=VECTOR('',#9307,0.165);
#2625=VECTOR('',#9316,0.6);
#2626=VECTOR('',#9329,0.225);
#2627=VECTOR('',#9336,1.);
#2628=VECTOR('',#9349,0.225);
#2629=VECTOR('',#9356,1.);
#2630=VECTOR('',#9367,1.);
#2631=VECTOR('',#9368,1.);
#2632=VECTOR('',#9369,1.);
#2633=VECTOR('',#9370,1.);
#2634=VECTOR('',#9371,1.);
#2635=VECTOR('',#9372,1.);
#2636=VECTOR('',#9373,1.);
#2637=VECTOR('',#9374,1.);
#2638=VECTOR('',#9377,1.);
#2639=VECTOR('',#9378,1.);
#2640=VECTOR('',#9379,1.);
#2641=VECTOR('',#9382,1.);
#2642=VECTOR('',#9383,1.);
#2643=VECTOR('',#9386,1.);
#2644=VECTOR('',#9387,1.);
#2645=VECTOR('',#9390,1.);
#2646=VECTOR('',#9391,1.);
#2647=VECTOR('',#9394,1.);
#2648=VECTOR('',#9395,1.);
#2649=VECTOR('',#9396,1.);
#2650=VECTOR('',#9397,1.);
#2651=VECTOR('',#9400,1.);
#2652=VECTOR('',#9403,1.);
#2653=VECTOR('',#9406,1.);
#2654=VECTOR('',#9419,0.325);
#2655=VECTOR('',#9424,0.35);
#2656=VECTOR('',#9429,0.335);
#2657=VECTOR('',#9438,0.21);
#2658=VECTOR('',#9443,0.2);
#2659=VECTOR('',#9448,0.18);
#2660=VECTOR('',#9453,1.);
#2661=VECTOR('',#9454,1.);
#2662=VECTOR('',#9455,1.);
#2663=VECTOR('',#9456,1.);
#2664=VECTOR('',#9459,1.);
#2665=VECTOR('',#9460,1.);
#2666=VECTOR('',#9461,1.);
#2667=VECTOR('',#9464,1.);
#2668=VECTOR('',#9465,1.);
#2669=VECTOR('',#9466,1.);
#2670=VECTOR('',#9469,1.);
#2671=VECTOR('',#9470,1.);
#2672=VECTOR('',#9471,1.);
#2673=VECTOR('',#9474,1.);
#2674=VECTOR('',#9475,1.);
#2675=VECTOR('',#9476,1.);
#2676=VECTOR('',#9479,1.);
#2677=VECTOR('',#9480,1.);
#2678=VECTOR('',#9609,0.425);
#2679=VECTOR('',#9614,1.);
#2680=VECTOR('',#9615,1.);
#2681=VECTOR('',#9616,1.);
#2682=VECTOR('',#9617,1.);
#2683=VECTOR('',#9620,1.);
#2684=VECTOR('',#9621,1.);
#2685=VECTOR('',#9622,1.);
#2686=VECTOR('',#9625,1.);
#2687=VECTOR('',#9626,1.);
#2688=VECTOR('',#9627,1.);
#2689=VECTOR('',#9630,1.);
#2690=VECTOR('',#9631,1.);
#2691=VECTOR('',#9642,0.275);
#2692=VECTOR('',#9649,0.275);
#2693=VECTOR('',#9656,0.275);
#2694=VECTOR('',#9663,0.275);
#2695=VECTOR('',#9668,1.);
#2696=VECTOR('',#9669,1.);
#2697=VECTOR('',#9670,1.);
#2698=VECTOR('',#9671,1.);
#2699=VECTOR('',#9676,1.);
#2700=VECTOR('',#9677,1.);
#2701=VECTOR('',#9678,1.);
#2702=VECTOR('',#9681,1.);
#2703=VECTOR('',#9682,1.);
#2704=VECTOR('',#9685,1.);
#2705=VECTOR('',#9686,1.);
#2706=VECTOR('',#9689,1.);
#2707=VECTOR('',#9696,0.5);
#2708=VECTOR('',#9703,0.6);
#2709=VECTOR('',#9714,0.605);
#2710=VECTOR('',#9721,1.25);
#2711=CIRCLE('',#6857,0.21);
#2712=CIRCLE('',#6858,0.21);
#2713=CIRCLE('',#6860,0.21);
#2714=CIRCLE('',#6861,0.21);
#2715=CIRCLE('',#6863,0.165);
#2716=CIRCLE('',#6864,0.165);
#2717=CIRCLE('',#6866,0.165);
#2718=CIRCLE('',#6867,0.165);
#2719=CIRCLE('',#6869,0.165);
#2720=CIRCLE('',#6870,0.165);
#2721=CIRCLE('',#6872,0.165);
#2722=CIRCLE('',#6873,0.165);
#2723=CIRCLE('',#6901,0.225);
#2724=CIRCLE('',#6902,0.225);
#2725=CIRCLE('',#6904,0.225);
#2726=CIRCLE('',#6905,0.225);
#2727=CIRCLE('',#6907,0.165);
#2728=CIRCLE('',#6908,0.165);
#2729=CIRCLE('',#6910,0.165);
#2730=CIRCLE('',#6911,0.165);
#2731=CIRCLE('',#6913,0.165);
#2732=CIRCLE('',#6914,0.165);
#2733=CIRCLE('',#6916,0.165);
#2734=CIRCLE('',#6917,0.165);
#2735=CIRCLE('',#6919,1.6);
#2736=CIRCLE('',#6920,1.6);
#2737=CIRCLE('',#6933,0.225);
#2738=CIRCLE('',#6934,0.225);
#2739=CIRCLE('',#6936,0.225);
#2740=CIRCLE('',#6937,0.225);
#2741=CIRCLE('',#6939,0.225);
#2742=CIRCLE('',#6940,0.225);
#2743=CIRCLE('',#6942,0.225);
#2744=CIRCLE('',#6943,0.225);
#2745=CIRCLE('',#6945,1.59);
#2746=CIRCLE('',#6946,1.59);
#2747=CIRCLE('',#6948,1.005);
#2748=CIRCLE('',#6950,1.005);
#2749=CIRCLE('',#6952,2.4);
#2750=CIRCLE('',#6953,2.4);
#2751=CIRCLE('',#6958,0.225);
#2752=CIRCLE('',#6959,0.225);
#2753=CIRCLE('',#6961,0.225);
#2754=CIRCLE('',#6962,0.225);
#2755=CIRCLE('',#6964,0.225);
#2756=CIRCLE('',#6965,0.225);
#2757=CIRCLE('',#6967,0.225);
#2758=CIRCLE('',#6968,0.225);
#2759=CIRCLE('',#6970,1.59);
#2760=CIRCLE('',#6971,1.59);
#2761=CIRCLE('',#6973,1.005);
#2762=CIRCLE('',#6975,1.005);
#2763=CIRCLE('',#6977,2.4);
#2764=CIRCLE('',#6978,2.4);
#2765=CIRCLE('',#6983,0.225);
#2766=CIRCLE('',#6984,0.225);
#2767=CIRCLE('',#6986,0.225);
#2768=CIRCLE('',#6987,0.225);
#2769=CIRCLE('',#6989,0.165);
#2770=CIRCLE('',#6990,0.165);
#2771=CIRCLE('',#6992,0.165);
#2772=CIRCLE('',#6993,0.165);
#2773=CIRCLE('',#6995,0.165);
#2774=CIRCLE('',#6996,0.165);
#2775=CIRCLE('',#6998,0.165);
#2776=CIRCLE('',#6999,0.165);
#2777=CIRCLE('',#7001,1.6);
#2778=CIRCLE('',#7002,1.6);
#2779=CIRCLE('',#7015,0.225);
#2780=CIRCLE('',#7016,0.225);
#2781=CIRCLE('',#7018,0.225);
#2782=CIRCLE('',#7019,0.225);
#2783=CIRCLE('',#7021,0.225);
#2784=CIRCLE('',#7022,0.225);
#2785=CIRCLE('',#7024,0.225);
#2786=CIRCLE('',#7025,0.225);
#2787=CIRCLE('',#7027,1.59);
#2788=CIRCLE('',#7028,1.59);
#2789=CIRCLE('',#7030,1.005);
#2790=CIRCLE('',#7032,1.005);
#2791=CIRCLE('',#7034,2.4);
#2792=CIRCLE('',#7035,2.4);
#2793=CIRCLE('',#7040,0.225);
#2794=CIRCLE('',#7041,0.225);
#2795=CIRCLE('',#7043,0.225);
#2796=CIRCLE('',#7044,0.225);
#2797=CIRCLE('',#7046,0.225);
#2798=CIRCLE('',#7047,0.225);
#2799=CIRCLE('',#7049,0.225);
#2800=CIRCLE('',#7050,0.225);
#2801=CIRCLE('',#7052,1.59);
#2802=CIRCLE('',#7053,1.59);
#2803=CIRCLE('',#7055,1.005);
#2804=CIRCLE('',#7057,1.005);
#2805=CIRCLE('',#7059,2.4);
#2806=CIRCLE('',#7060,2.4);
#2807=CIRCLE('',#7065,0.165);
#2808=CIRCLE('',#7066,0.165);
#2809=CIRCLE('',#7069,0.165);
#2810=CIRCLE('',#7070,0.165);
#2811=CIRCLE('',#7073,0.165);
#2812=CIRCLE('',#7074,0.165);
#2813=CIRCLE('',#7077,0.165);
#2814=CIRCLE('',#7078,0.165);
#2815=CIRCLE('',#7081,1.05);
#2816=CIRCLE('',#7082,1.05);
#2817=CIRCLE('',#7084,0.625);
#2818=CIRCLE('',#7086,0.625);
#2819=CIRCLE('',#7088,0.5);
#2820=CIRCLE('',#7089,0.5);
#2821=CIRCLE('',#7091,0.275);
#2822=CIRCLE('',#7093,0.275);
#2823=CIRCLE('',#7095,0.5);
#2824=CIRCLE('',#7096,0.5);
#2825=CIRCLE('',#7098,0.275);
#2826=CIRCLE('',#7100,0.275);
#2827=CIRCLE('',#7117,0.625);
#2828=CIRCLE('',#7118,0.625);
#2829=CIRCLE('',#7120,1.04);
#2830=CIRCLE('',#7121,1.04);
#2831=CIRCLE('',#7126,0.225);
#2832=CIRCLE('',#7127,0.225);
#2833=CIRCLE('',#7129,0.225);
#2834=CIRCLE('',#7130,0.225);
#2835=CIRCLE('',#7132,0.225);
#2836=CIRCLE('',#7133,0.225);
#2837=CIRCLE('',#7135,0.225);
#2838=CIRCLE('',#7136,0.225);
#2839=CIRCLE('',#7138,1.04);
#2840=CIRCLE('',#7139,1.04);
#2841=CIRCLE('',#7141,0.625);
#2842=CIRCLE('',#7143,0.625);
#2843=CIRCLE('',#7145,1.8);
#2844=CIRCLE('',#7146,1.8);
#2845=CIRCLE('',#7150,0.075);
#2846=CIRCLE('',#7151,0.075);
#2847=CIRCLE('',#7157,1.070235);
#2848=CIRCLE('',#7158,1.070235);
#2849=CIRCLE('',#7159,0.309556);
#2850=CIRCLE('',#7160,1.070235);
#2851=CIRCLE('',#7161,1.070235);
#2852=CIRCLE('',#7163,1.070235);
#2853=CIRCLE('',#7165,0.6);
#2854=CIRCLE('',#7166,0.6);
#2855=CIRCLE('',#7168,0.66);
#2856=CIRCLE('',#7171,1.070235);
#2857=CIRCLE('',#7173,0.66);
#2858=CIRCLE('',#7177,1.129765);
#2859=CIRCLE('',#7178,1.129765);
#2860=CIRCLE('',#7179,0.309556);
#2861=CIRCLE('',#7180,1.129765);
#2862=CIRCLE('',#7181,1.129765);
#2863=CIRCLE('',#7183,1.129765);
#2864=CIRCLE('',#7185,1.54);
#2865=CIRCLE('',#7186,1.129765);
#2866=CIRCLE('',#7188,1.6);
#2867=CIRCLE('',#7190,1.6);
#2868=CIRCLE('',#7192,1.54);
#2869=CIRCLE('',#7197,0.29765);
#2870=CIRCLE('',#7199,0.29765);
#2871=CIRCLE('',#7201,0.29765);
#2872=CIRCLE('',#7203,0.29765);
#2873=CIRCLE('',#7205,0.29765);
#2874=CIRCLE('',#7207,0.29765);
#2875=CIRCLE('',#7209,0.29765);
#2876=CIRCLE('',#7212,0.303778037777585);
#2877=CIRCLE('',#7213,0.303778037777585);
#2878=CIRCLE('',#7215,1.123812);
#2879=CIRCLE('',#7216,1.123812);
#2880=CIRCLE('',#7217,1.123812);
#2881=CIRCLE('',#7218,1.123812);
#2882=CIRCLE('',#7219,1.123812);
#2883=CIRCLE('',#7220,1.123812);
#2884=CIRCLE('',#7221,1.123812);
#2885=CIRCLE('',#7222,1.123812);
#2886=CIRCLE('',#7223,1.123812);
#2887=CIRCLE('',#7225,1.076188);
#2888=CIRCLE('',#7226,0.303778037777585);
#2889=CIRCLE('',#7228,0.303778037777585);
#2890=CIRCLE('',#7230,1.076188);
#2891=CIRCLE('',#7231,0.303778037777585);
#2892=CIRCLE('',#7233,0.303778037777585);
#2893=CIRCLE('',#7235,1.076188);
#2894=CIRCLE('',#7236,1.076188);
#2895=CIRCLE('',#7237,0.303778037777585);
#2896=CIRCLE('',#7239,0.303778037777585);
#2897=CIRCLE('',#7241,1.076188);
#2898=CIRCLE('',#7242,0.303778037777585);
#2899=CIRCLE('',#7244,0.303778037777585);
#2900=CIRCLE('',#7246,1.076188);
#2901=CIRCLE('',#7247,0.303778037777585);
#2902=CIRCLE('',#7249,0.303778037777585);
#2903=CIRCLE('',#7251,1.076188);
#2904=CIRCLE('',#7252,1.076188);
#2905=CIRCLE('',#7253,1.076188);
#2906=CIRCLE('',#7255,0.303778037777585);
#2907=CIRCLE('',#7257,0.303778037777585);
#2908=CIRCLE('',#7262,1.119765);
#2909=CIRCLE('',#7263,1.085235);
#2910=CIRCLE('',#7265,1.119765);
#2911=CIRCLE('',#7267,1.085235);
#2912=CIRCLE('',#7270,1.119765);
#2913=CIRCLE('',#7271,1.085235);
#2914=CIRCLE('',#7273,1.119765);
#2915=CIRCLE('',#7275,1.085235);
#2916=CIRCLE('',#7284,0.375);
#2917=CIRCLE('',#7286,0.425);
#2918=CIRCLE('',#7288,0.425);
#2919=CIRCLE('',#7290,0.395);
#2920=CIRCLE('',#7292,0.27);
#2921=CIRCLE('',#7294,0.24505);
#2922=CIRCLE('',#7296,0.24505);
#2923=CIRCLE('',#7298,0.2);
#2924=CIRCLE('',#7311,0.9);
#2925=CIRCLE('',#7314,0.9);
#2926=CIRCLE('',#7318,1.05);
#2927=CIRCLE('',#7319,0.9);
#2928=CIRCLE('',#7321,1.05);
#2929=CIRCLE('',#7323,1.);
#2930=CIRCLE('',#7325,1.);
#2931=CIRCLE('',#7327,1.05);
#2932=CIRCLE('',#7329,1.05);
#2933=CIRCLE('',#7331,1.);
#2934=CIRCLE('',#7333,1.);
#2935=CIRCLE('',#7335,1.05);
#2936=CIRCLE('',#7337,1.05);
#2937=CIRCLE('',#7339,0.9);
#2938=CIRCLE('',#7343,0.895);
#2939=CIRCLE('',#7344,0.605);
#2940=CIRCLE('',#7347,0.895);
#2941=CIRCLE('',#7348,0.605);
#2942=CIRCLE('',#7351,0.895);
#2943=CIRCLE('',#7352,0.605);
#2944=CIRCLE('',#7354,0.895);
#2945=CIRCLE('',#7356,0.605);
#2946=CIRCLE('',#7370,0.1954);
#2947=CIRCLE('',#7372,0.3);
#2948=CIRCLE('',#7374,0.35);
#2949=CIRCLE('',#7376,0.35);
#2950=CIRCLE('',#7378,0.32);
#2951=CIRCLE('',#7380,0.22);
#2952=CIRCLE('',#7382,0.1954);
#2953=CIRCLE('',#7387,0.165);
#2954=CIRCLE('',#7388,0.165);
#2955=CIRCLE('',#7391,0.165);
#2956=CIRCLE('',#7392,0.165);
#2957=CIRCLE('',#7396,0.6);
#2958=CIRCLE('',#7400,0.6);
#2959=CIRCLE('',#7403,0.6);
#2960=CIRCLE('',#7407,0.6);
#2961=CIRCLE('',#7409,0.6);
#2962=CIRCLE('',#7410,0.6);
#2963=CIRCLE('',#7415,0.605);
#2964=CIRCLE('',#7416,0.605);
#2965=CIRCLE('',#7418,0.8);
#2966=CIRCLE('',#7419,0.8);
#2967=CIRCLE('',#7424,0.605);
#2968=CIRCLE('',#7425,0.605);
#2969=CIRCLE('',#7427,0.8);
#2970=CIRCLE('',#7428,0.8);
#2971=CIRCLE('',#7433,0.605);
#2972=CIRCLE('',#7434,0.605);
#2973=CIRCLE('',#7436,0.8);
#2974=CIRCLE('',#7437,0.8);
#2975=CIRCLE('',#7442,0.605);
#2976=CIRCLE('',#7443,0.605);
#2977=CIRCLE('',#7445,0.8);
#2978=CIRCLE('',#7446,0.8);
#2979=CIRCLE('',#7454,0.9);
#2980=CIRCLE('',#7455,0.6);
#2981=CIRCLE('',#7457,0.6);
#2982=CIRCLE('',#7459,0.9);
#2983=CIRCLE('',#7460,0.9);
#2984=CIRCLE('',#7462,0.9);
#2985=CIRCLE('',#7465,2.);
#2986=CIRCLE('',#7466,2.);
#2987=CIRCLE('',#7471,0.225);
#2988=CIRCLE('',#7472,0.225);
#2989=CIRCLE('',#7477,1.2);
#2990=CIRCLE('',#7478,0.6);
#2991=CIRCLE('',#7480,0.6);
#2992=CIRCLE('',#7482,0.7);
#2993=CIRCLE('',#7483,0.7);
#2994=CIRCLE('',#7485,1.2);
#2995=CIRCLE('',#7489,1.2);
#2996=CIRCLE('',#7491,1.2);
#2997=CIRCLE('',#7495,0.165);
#2998=CIRCLE('',#7496,0.165);
#2999=CIRCLE('',#7499,0.6);
#3000=CIRCLE('',#7500,0.6);
#3001=CIRCLE('',#7505,0.225);
#3002=CIRCLE('',#7506,0.225);
#3003=CIRCLE('',#7508,1.);
#3004=CIRCLE('',#7509,1.);
#3005=CIRCLE('',#7514,0.225);
#3006=CIRCLE('',#7515,0.225);
#3007=CIRCLE('',#7517,1.);
#3008=CIRCLE('',#7518,1.);
#3009=CIRCLE('',#7534,0.3);
#3010=CIRCLE('',#7536,0.35);
#3011=CIRCLE('',#7538,0.35);
#3012=CIRCLE('',#7540,0.32);
#3013=CIRCLE('',#7542,0.22);
#3014=CIRCLE('',#7544,0.1954);
#3015=CIRCLE('',#7546,0.1954);
#3016=CIRCLE('',#7548,0.16);
#3017=CIRCLE('',#7619,0.425);
#3018=CIRCLE('',#7620,0.425);
#3019=CIRCLE('',#7629,0.275);
#3020=CIRCLE('',#7630,0.275);
#3021=CIRCLE('',#7632,0.275);
#3022=CIRCLE('',#7633,0.275);
#3023=CIRCLE('',#7635,0.275);
#3024=CIRCLE('',#7636,0.275);
#3025=CIRCLE('',#7638,0.275);
#3026=CIRCLE('',#7639,0.275);
#3027=CIRCLE('',#7641,0.6);
#3028=CIRCLE('',#7648,0.5);
#3029=CIRCLE('',#7649,0.5);
#3030=CIRCLE('',#7652,0.6);
#3031=CIRCLE('',#7656,0.605);
#3032=CIRCLE('',#7657,0.605);
#3033=CIRCLE('',#7659,1.25);
#3034=CIRCLE('',#7660,1.25);
#3035=VERTEX_POINT('',#9744);
#3036=VERTEX_POINT('',#9746);
#3037=VERTEX_POINT('',#9750);
#3038=VERTEX_POINT('',#9752);
#3039=VERTEX_POINT('',#9756);
#3040=VERTEX_POINT('',#9758);
#3041=VERTEX_POINT('',#9762);
#3042=VERTEX_POINT('',#9764);
#3043=VERTEX_POINT('',#9768);
#3044=VERTEX_POINT('',#9770);
#3045=VERTEX_POINT('',#9774);
#3046=VERTEX_POINT('',#9776);
#3047=VERTEX_POINT('',#9780);
#3048=VERTEX_POINT('',#9781);
#3049=VERTEX_POINT('',#9783);
#3050=VERTEX_POINT('',#9785);
#3051=VERTEX_POINT('',#9789);
#3052=VERTEX_POINT('',#9791);
#3053=VERTEX_POINT('',#9795);
#3054=VERTEX_POINT('',#9797);
#3055=VERTEX_POINT('',#9805);
#3056=VERTEX_POINT('',#9806);
#3057=VERTEX_POINT('',#9808);
#3058=VERTEX_POINT('',#9810);
#3059=VERTEX_POINT('',#9814);
#3060=VERTEX_POINT('',#9816);
#3061=VERTEX_POINT('',#9820);
#3062=VERTEX_POINT('',#9822);
#3063=VERTEX_POINT('',#9832);
#3064=VERTEX_POINT('',#9833);
#3065=VERTEX_POINT('',#9835);
#3066=VERTEX_POINT('',#9837);
#3067=VERTEX_POINT('',#9841);
#3068=VERTEX_POINT('',#9843);
#3069=VERTEX_POINT('',#9847);
#3070=VERTEX_POINT('',#9849);
#3071=VERTEX_POINT('',#9859);
#3072=VERTEX_POINT('',#9860);
#3073=VERTEX_POINT('',#9862);
#3074=VERTEX_POINT('',#9864);
#3075=VERTEX_POINT('',#9868);
#3076=VERTEX_POINT('',#9870);
#3077=VERTEX_POINT('',#9874);
#3078=VERTEX_POINT('',#9876);
#3079=VERTEX_POINT('',#9886);
#3080=VERTEX_POINT('',#9888);
#3081=VERTEX_POINT('',#9892);
#3082=VERTEX_POINT('',#9894);
#3083=VERTEX_POINT('',#9898);
#3084=VERTEX_POINT('',#9900);
#3085=VERTEX_POINT('',#9904);
#3086=VERTEX_POINT('',#9906);
#3087=VERTEX_POINT('',#9910);
#3088=VERTEX_POINT('',#9912);
#3089=VERTEX_POINT('',#9916);
#3090=VERTEX_POINT('',#9918);
#3091=VERTEX_POINT('',#9922);
#3092=VERTEX_POINT('',#9924);
#3093=VERTEX_POINT('',#9928);
#3094=VERTEX_POINT('',#9929);
#3095=VERTEX_POINT('',#9931);
#3096=VERTEX_POINT('',#9933);
#3097=VERTEX_POINT('',#9937);
#3098=VERTEX_POINT('',#9938);
#3099=VERTEX_POINT('',#9940);
#3100=VERTEX_POINT('',#9942);
#3101=VERTEX_POINT('',#9946);
#3102=VERTEX_POINT('',#9948);
#3103=VERTEX_POINT('',#9952);
#3104=VERTEX_POINT('',#9954);
#3105=VERTEX_POINT('',#9958);
#3106=VERTEX_POINT('',#9960);
#3107=VERTEX_POINT('',#9965);
#3108=VERTEX_POINT('',#9969);
#3109=VERTEX_POINT('',#9979);
#3110=VERTEX_POINT('',#9981);
#3111=VERTEX_POINT('',#9985);
#3112=VERTEX_POINT('',#9987);
#3113=VERTEX_POINT('',#9991);
#3114=VERTEX_POINT('',#9993);
#3115=VERTEX_POINT('',#9997);
#3116=VERTEX_POINT('',#9999);
#3117=VERTEX_POINT('',#10003);
#3118=VERTEX_POINT('',#10005);
#3119=VERTEX_POINT('',#10009);
#3120=VERTEX_POINT('',#10012);
#3121=VERTEX_POINT('',#10016);
#3122=VERTEX_POINT('',#10018);
#3123=VERTEX_POINT('',#10025);
#3124=VERTEX_POINT('',#10027);
#3125=VERTEX_POINT('',#10031);
#3126=VERTEX_POINT('',#10033);
#3127=VERTEX_POINT('',#10037);
#3128=VERTEX_POINT('',#10039);
#3129=VERTEX_POINT('',#10043);
#3130=VERTEX_POINT('',#10045);
#3131=VERTEX_POINT('',#10049);
#3132=VERTEX_POINT('',#10051);
#3133=VERTEX_POINT('',#10055);
#3134=VERTEX_POINT('',#10058);
#3135=VERTEX_POINT('',#10062);
#3136=VERTEX_POINT('',#10064);
#3137=VERTEX_POINT('',#10071);
#3138=VERTEX_POINT('',#10073);
#3139=VERTEX_POINT('',#10077);
#3140=VERTEX_POINT('',#10079);
#3141=VERTEX_POINT('',#10083);
#3142=VERTEX_POINT('',#10085);
#3143=VERTEX_POINT('',#10089);
#3144=VERTEX_POINT('',#10091);
#3145=VERTEX_POINT('',#10095);
#3146=VERTEX_POINT('',#10097);
#3147=VERTEX_POINT('',#10101);
#3148=VERTEX_POINT('',#10103);
#3149=VERTEX_POINT('',#10107);
#3150=VERTEX_POINT('',#10109);
#3151=VERTEX_POINT('',#10113);
#3152=VERTEX_POINT('',#10114);
#3153=VERTEX_POINT('',#10116);
#3154=VERTEX_POINT('',#10118);
#3155=VERTEX_POINT('',#10122);
#3156=VERTEX_POINT('',#10123);
#3157=VERTEX_POINT('',#10125);
#3158=VERTEX_POINT('',#10127);
#3159=VERTEX_POINT('',#10131);
#3160=VERTEX_POINT('',#10133);
#3161=VERTEX_POINT('',#10137);
#3162=VERTEX_POINT('',#10139);
#3163=VERTEX_POINT('',#10143);
#3164=VERTEX_POINT('',#10145);
#3165=VERTEX_POINT('',#10150);
#3166=VERTEX_POINT('',#10154);
#3167=VERTEX_POINT('',#10164);
#3168=VERTEX_POINT('',#10166);
#3169=VERTEX_POINT('',#10170);
#3170=VERTEX_POINT('',#10172);
#3171=VERTEX_POINT('',#10176);
#3172=VERTEX_POINT('',#10178);
#3173=VERTEX_POINT('',#10182);
#3174=VERTEX_POINT('',#10184);
#3175=VERTEX_POINT('',#10188);
#3176=VERTEX_POINT('',#10190);
#3177=VERTEX_POINT('',#10194);
#3178=VERTEX_POINT('',#10197);
#3179=VERTEX_POINT('',#10201);
#3180=VERTEX_POINT('',#10203);
#3181=VERTEX_POINT('',#10210);
#3182=VERTEX_POINT('',#10212);
#3183=VERTEX_POINT('',#10216);
#3184=VERTEX_POINT('',#10218);
#3185=VERTEX_POINT('',#10222);
#3186=VERTEX_POINT('',#10224);
#3187=VERTEX_POINT('',#10228);
#3188=VERTEX_POINT('',#10230);
#3189=VERTEX_POINT('',#10234);
#3190=VERTEX_POINT('',#10236);
#3191=VERTEX_POINT('',#10240);
#3192=VERTEX_POINT('',#10243);
#3193=VERTEX_POINT('',#10247);
#3194=VERTEX_POINT('',#10249);
#3195=VERTEX_POINT('',#10256);
#3196=VERTEX_POINT('',#10258);
#3197=VERTEX_POINT('',#10263);
#3198=VERTEX_POINT('',#10265);
#3199=VERTEX_POINT('',#10270);
#3200=VERTEX_POINT('',#10272);
#3201=VERTEX_POINT('',#10277);
#3202=VERTEX_POINT('',#10279);
#3203=VERTEX_POINT('',#10284);
#3204=VERTEX_POINT('',#10286);
#3205=VERTEX_POINT('',#10290);
#3206=VERTEX_POINT('',#10293);
#3207=VERTEX_POINT('',#10297);
#3208=VERTEX_POINT('',#10299);
#3209=VERTEX_POINT('',#10303);
#3210=VERTEX_POINT('',#10306);
#3211=VERTEX_POINT('',#10310);
#3212=VERTEX_POINT('',#10312);
#3213=VERTEX_POINT('',#10316);
#3214=VERTEX_POINT('',#10319);
#3215=VERTEX_POINT('',#10323);
#3216=VERTEX_POINT('',#10324);
#3217=VERTEX_POINT('',#10326);
#3218=VERTEX_POINT('',#10328);
#3219=VERTEX_POINT('',#10330);
#3220=VERTEX_POINT('',#10332);
#3221=VERTEX_POINT('',#10334);
#3222=VERTEX_POINT('',#10336);
#3223=VERTEX_POINT('',#10338);
#3224=VERTEX_POINT('',#10340);
#3225=VERTEX_POINT('',#10342);
#3226=VERTEX_POINT('',#10344);
#3227=VERTEX_POINT('',#10348);
#3228=VERTEX_POINT('',#10349);
#3229=VERTEX_POINT('',#10354);
#3230=VERTEX_POINT('',#10355);
#3231=VERTEX_POINT('',#10360);
#3232=VERTEX_POINT('',#10362);
#3233=VERTEX_POINT('',#10366);
#3234=VERTEX_POINT('',#10370);
#3235=VERTEX_POINT('',#10378);
#3236=VERTEX_POINT('',#10380);
#3237=VERTEX_POINT('',#10384);
#3238=VERTEX_POINT('',#10388);
#3239=VERTEX_POINT('',#10398);
#3240=VERTEX_POINT('',#10400);
#3241=VERTEX_POINT('',#10404);
#3242=VERTEX_POINT('',#10406);
#3243=VERTEX_POINT('',#10413);
#3244=VERTEX_POINT('',#10415);
#3245=VERTEX_POINT('',#10419);
#3246=VERTEX_POINT('',#10421);
#3247=VERTEX_POINT('',#10425);
#3248=VERTEX_POINT('',#10427);
#3249=VERTEX_POINT('',#10431);
#3250=VERTEX_POINT('',#10433);
#3251=VERTEX_POINT('',#10437);
#3252=VERTEX_POINT('',#10439);
#3253=VERTEX_POINT('',#10443);
#3254=VERTEX_POINT('',#10446);
#3255=VERTEX_POINT('',#10450);
#3256=VERTEX_POINT('',#10452);
#3257=VERTEX_POINT('',#11698);
#3258=VERTEX_POINT('',#11700);
#3259=VERTEX_POINT('',#11831);
#3260=VERTEX_POINT('',#11832);
#3261=VERTEX_POINT('',#11835);
#3262=VERTEX_POINT('',#11837);
#3263=VERTEX_POINT('',#11841);
#3264=VERTEX_POINT('',#11845);
#3265=VERTEX_POINT('',#11847);
#3266=VERTEX_POINT('',#11851);
#3267=VERTEX_POINT('',#11856);
#3268=VERTEX_POINT('',#11860);
#3269=VERTEX_POINT('',#11866);
#3270=VERTEX_POINT('',#11867);
#3271=VERTEX_POINT('',#11870);
#3272=VERTEX_POINT('',#11872);
#3273=VERTEX_POINT('',#11876);
#3274=VERTEX_POINT('',#11880);
#3275=VERTEX_POINT('',#11882);
#3276=VERTEX_POINT('',#11885);
#3277=VERTEX_POINT('',#11889);
#3278=VERTEX_POINT('',#11893);
#3279=VERTEX_POINT('',#11901);
#3280=VERTEX_POINT('',#11902);
#3281=VERTEX_POINT('',#11905);
#3282=VERTEX_POINT('',#11906);
#3283=VERTEX_POINT('',#11909);
#3284=VERTEX_POINT('',#11910);
#3285=VERTEX_POINT('',#11913);
#3286=VERTEX_POINT('',#11914);
#3287=VERTEX_POINT('',#11917);
#3288=VERTEX_POINT('',#11918);
#3289=VERTEX_POINT('',#11921);
#3290=VERTEX_POINT('',#11922);
#3291=VERTEX_POINT('',#11925);
#3292=VERTEX_POINT('',#11926);
#3293=VERTEX_POINT('',#11930);
#3294=VERTEX_POINT('',#11931);
#3295=VERTEX_POINT('',#11954);
#3296=VERTEX_POINT('',#11956);
#3297=VERTEX_POINT('',#11981);
#3298=VERTEX_POINT('',#11983);
#3299=VERTEX_POINT('',#12006);
#3300=VERTEX_POINT('',#12008);
#3301=VERTEX_POINT('',#12031);
#3302=VERTEX_POINT('',#12033);
#3303=VERTEX_POINT('',#12036);
#3304=VERTEX_POINT('',#12038);
#3305=VERTEX_POINT('',#12061);
#3306=VERTEX_POINT('',#12063);
#3307=VERTEX_POINT('',#12086);
#3308=VERTEX_POINT('',#12088);
#3309=VERTEX_POINT('',#12111);
#3310=VERTEX_POINT('',#12113);
#3311=VERTEX_POINT('',#12138);
#3312=VERTEX_POINT('',#12142);
#3313=VERTEX_POINT('',#12167);
#3314=VERTEX_POINT('',#12171);
#3315=VERTEX_POINT('',#12196);
#3316=VERTEX_POINT('',#12198);
#3317=VERTEX_POINT('',#12202);
#3318=VERTEX_POINT('',#12227);
#3319=VERTEX_POINT('',#12231);
#3320=VERTEX_POINT('',#12256);
#3321=VERTEX_POINT('',#12260);
#3322=VERTEX_POINT('',#12285);
#3323=VERTEX_POINT('',#12288);
#3324=VERTEX_POINT('',#12290);
#3325=VERTEX_POINT('',#12322);
#3326=VERTEX_POINT('',#12324);
#3327=VERTEX_POINT('',#12327);
#3328=VERTEX_POINT('',#12331);
#3329=VERTEX_POINT('',#12336);
#3330=VERTEX_POINT('',#12338);
#3331=VERTEX_POINT('',#12341);
#3332=VERTEX_POINT('',#12345);
#3333=VERTEX_POINT('',#12356);
#3334=VERTEX_POINT('',#12359);
#3335=VERTEX_POINT('',#12363);
#3336=VERTEX_POINT('',#12367);
#3337=VERTEX_POINT('',#12371);
#3338=VERTEX_POINT('',#12374);
#3339=VERTEX_POINT('',#12378);
#3340=VERTEX_POINT('',#12382);
#3341=VERTEX_POINT('',#12387);
#3342=VERTEX_POINT('',#12388);
#3343=VERTEX_POINT('',#12390);
#3344=VERTEX_POINT('',#12392);
#3345=VERTEX_POINT('',#12396);
#3346=VERTEX_POINT('',#12398);
#3347=VERTEX_POINT('',#12402);
#3348=VERTEX_POINT('',#12404);
#3349=VERTEX_POINT('',#12408);
#3350=VERTEX_POINT('',#12410);
#3351=VERTEX_POINT('',#12414);
#3352=VERTEX_POINT('',#12416);
#3353=VERTEX_POINT('',#12427);
#3354=VERTEX_POINT('',#12428);
#3355=VERTEX_POINT('',#12430);
#3356=VERTEX_POINT('',#12432);
#3357=VERTEX_POINT('',#12436);
#3358=VERTEX_POINT('',#12438);
#3359=VERTEX_POINT('',#12442);
#3360=VERTEX_POINT('',#12444);
#3361=VERTEX_POINT('',#12452);
#3362=VERTEX_POINT('',#12454);
#3363=VERTEX_POINT('',#12457);
#3364=VERTEX_POINT('',#12461);
#3365=VERTEX_POINT('',#12464);
#3366=VERTEX_POINT('',#12468);
#3367=VERTEX_POINT('',#12471);
#3368=VERTEX_POINT('',#12475);
#3369=VERTEX_POINT('',#12478);
#3370=VERTEX_POINT('',#12482);
#3371=VERTEX_POINT('',#12485);
#3372=VERTEX_POINT('',#12489);
#3373=VERTEX_POINT('',#12495);
#3374=VERTEX_POINT('',#12496);
#3375=VERTEX_POINT('',#12498);
#3376=VERTEX_POINT('',#12500);
#3377=VERTEX_POINT('',#12504);
#3378=VERTEX_POINT('',#12506);
#3379=VERTEX_POINT('',#12510);
#3380=VERTEX_POINT('',#12512);
#3381=VERTEX_POINT('',#12519);
#3382=VERTEX_POINT('',#12521);
#3383=VERTEX_POINT('',#12524);
#3384=VERTEX_POINT('',#12528);
#3385=VERTEX_POINT('',#12536);
#3386=VERTEX_POINT('',#12537);
#3387=VERTEX_POINT('',#12539);
#3388=VERTEX_POINT('',#12541);
#3389=VERTEX_POINT('',#12545);
#3390=VERTEX_POINT('',#12547);
#3391=VERTEX_POINT('',#12551);
#3392=VERTEX_POINT('',#12553);
#3393=VERTEX_POINT('',#12557);
#3394=VERTEX_POINT('',#12559);
#3395=VERTEX_POINT('',#12563);
#3396=VERTEX_POINT('',#12565);
#3397=VERTEX_POINT('',#12574);
#3398=VERTEX_POINT('',#12577);
#3399=VERTEX_POINT('',#12580);
#3400=VERTEX_POINT('',#12584);
#3401=VERTEX_POINT('',#12588);
#3402=VERTEX_POINT('',#12592);
#3403=VERTEX_POINT('',#12595);
#3404=VERTEX_POINT('',#12603);
#3405=VERTEX_POINT('',#12605);
#3406=VERTEX_POINT('',#12610);
#3407=VERTEX_POINT('',#12612);
#3408=VERTEX_POINT('',#12617);
#3409=VERTEX_POINT('',#12618);
#3410=VERTEX_POINT('',#12620);
#3411=VERTEX_POINT('',#12622);
#3412=VERTEX_POINT('',#12626);
#3413=VERTEX_POINT('',#12628);
#3414=VERTEX_POINT('',#12632);
#3415=VERTEX_POINT('',#12634);
#3416=VERTEX_POINT('',#12642);
#3417=VERTEX_POINT('',#12643);
#3418=VERTEX_POINT('',#12645);
#3419=VERTEX_POINT('',#12647);
#3420=VERTEX_POINT('',#12651);
#3421=VERTEX_POINT('',#12653);
#3422=VERTEX_POINT('',#12657);
#3423=VERTEX_POINT('',#12659);
#3424=VERTEX_POINT('',#12667);
#3425=VERTEX_POINT('',#12669);
#3426=VERTEX_POINT('',#12676);
#3427=VERTEX_POINT('',#12678);
#3428=VERTEX_POINT('',#12682);
#3429=VERTEX_POINT('',#12684);
#3430=VERTEX_POINT('',#12691);
#3431=VERTEX_POINT('',#12693);
#3432=VERTEX_POINT('',#12697);
#3433=VERTEX_POINT('',#12699);
#3434=VERTEX_POINT('',#12706);
#3435=VERTEX_POINT('',#12708);
#3436=VERTEX_POINT('',#12712);
#3437=VERTEX_POINT('',#12714);
#3438=VERTEX_POINT('',#12721);
#3439=VERTEX_POINT('',#12723);
#3440=VERTEX_POINT('',#12727);
#3441=VERTEX_POINT('',#12729);
#3442=VERTEX_POINT('',#12736);
#3443=VERTEX_POINT('',#12737);
#3444=VERTEX_POINT('',#12739);
#3445=VERTEX_POINT('',#12741);
#3446=VERTEX_POINT('',#12745);
#3447=VERTEX_POINT('',#12747);
#3448=VERTEX_POINT('',#12751);
#3449=VERTEX_POINT('',#12753);
#3450=VERTEX_POINT('',#12757);
#3451=VERTEX_POINT('',#12763);
#3452=VERTEX_POINT('',#12765);
#3453=VERTEX_POINT('',#12769);
#3454=VERTEX_POINT('',#12774);
#3455=VERTEX_POINT('',#12776);
#3456=VERTEX_POINT('',#12783);
#3457=VERTEX_POINT('',#12785);
#3458=VERTEX_POINT('',#12789);
#3459=VERTEX_POINT('',#12790);
#3460=VERTEX_POINT('',#12792);
#3461=VERTEX_POINT('',#12794);
#3462=VERTEX_POINT('',#12798);
#3463=VERTEX_POINT('',#12800);
#3464=VERTEX_POINT('',#12804);
#3465=VERTEX_POINT('',#12806);
#3466=VERTEX_POINT('',#12810);
#3467=VERTEX_POINT('',#12816);
#3468=VERTEX_POINT('',#12817);
#3469=VERTEX_POINT('',#12819);
#3470=VERTEX_POINT('',#12821);
#3471=VERTEX_POINT('',#12825);
#3472=VERTEX_POINT('',#12827);
#3473=VERTEX_POINT('',#12831);
#3474=VERTEX_POINT('',#12835);
#3475=VERTEX_POINT('',#12841);
#3476=VERTEX_POINT('',#12847);
#3477=VERTEX_POINT('',#12849);
#3478=VERTEX_POINT('',#12854);
#3479=VERTEX_POINT('',#12856);
#3480=VERTEX_POINT('',#12863);
#3481=VERTEX_POINT('',#12865);
#3482=VERTEX_POINT('',#12869);
#3483=VERTEX_POINT('',#12871);
#3484=VERTEX_POINT('',#12878);
#3485=VERTEX_POINT('',#12880);
#3486=VERTEX_POINT('',#12884);
#3487=VERTEX_POINT('',#12886);
#3488=VERTEX_POINT('',#12893);
#3489=VERTEX_POINT('',#12894);
#3490=VERTEX_POINT('',#12896);
#3491=VERTEX_POINT('',#12898);
#3492=VERTEX_POINT('',#12900);
#3493=VERTEX_POINT('',#12902);
#3494=VERTEX_POINT('',#12904);
#3495=VERTEX_POINT('',#12906);
#3496=VERTEX_POINT('',#12910);
#3497=VERTEX_POINT('',#12912);
#3498=VERTEX_POINT('',#12916);
#3499=VERTEX_POINT('',#12920);
#3500=VERTEX_POINT('',#12924);
#3501=VERTEX_POINT('',#12928);
#3502=VERTEX_POINT('',#12930);
#3503=VERTEX_POINT('',#12932);
#3504=VERTEX_POINT('',#12944);
#3505=VERTEX_POINT('',#12947);
#3506=VERTEX_POINT('',#12951);
#3507=VERTEX_POINT('',#12955);
#3508=VERTEX_POINT('',#12959);
#3509=VERTEX_POINT('',#12962);
#3510=VERTEX_POINT('',#12966);
#3511=VERTEX_POINT('',#12970);
#3512=VERTEX_POINT('',#12975);
#3513=VERTEX_POINT('',#12976);
#3514=VERTEX_POINT('',#12978);
#3515=VERTEX_POINT('',#12980);
#3516=VERTEX_POINT('',#12984);
#3517=VERTEX_POINT('',#12986);
#3518=VERTEX_POINT('',#12990);
#3519=VERTEX_POINT('',#12992);
#3520=VERTEX_POINT('',#12996);
#3521=VERTEX_POINT('',#12998);
#3522=VERTEX_POINT('',#13002);
#3523=VERTEX_POINT('',#13004);
#3524=VERTEX_POINT('',#13073);
#3525=VERTEX_POINT('',#13075);
#3526=VERTEX_POINT('',#13079);
#3527=VERTEX_POINT('',#13080);
#3528=VERTEX_POINT('',#13082);
#3529=VERTEX_POINT('',#13084);
#3530=VERTEX_POINT('',#13088);
#3531=VERTEX_POINT('',#13090);
#3532=VERTEX_POINT('',#13094);
#3533=VERTEX_POINT('',#13096);
#3534=VERTEX_POINT('',#13106);
#3535=VERTEX_POINT('',#13108);
#3536=VERTEX_POINT('',#13112);
#3537=VERTEX_POINT('',#13114);
#3538=VERTEX_POINT('',#13118);
#3539=VERTEX_POINT('',#13120);
#3540=VERTEX_POINT('',#13124);
#3541=VERTEX_POINT('',#13126);
#3542=VERTEX_POINT('',#13130);
#3543=VERTEX_POINT('',#13131);
#3544=VERTEX_POINT('',#13133);
#3545=VERTEX_POINT('',#13135);
#3546=VERTEX_POINT('',#13138);
#3547=VERTEX_POINT('',#13141);
#3548=VERTEX_POINT('',#13143);
#3549=VERTEX_POINT('',#13147);
#3550=VERTEX_POINT('',#13151);
#3551=VERTEX_POINT('',#13158);
#3552=VERTEX_POINT('',#13160);
#3553=VERTEX_POINT('',#13165);
#3554=VERTEX_POINT('',#13171);
#3555=VERTEX_POINT('',#13173);
#3556=VERTEX_POINT('',#13177);
#3557=VERTEX_POINT('',#13179);
#3558=EDGE_CURVE('',#3035,#3035,#2711,.T.);
#3559=EDGE_CURVE('',#3035,#3036,#1833,.T.);
#3560=EDGE_CURVE('',#3036,#3036,#2712,.T.);
#3561=EDGE_CURVE('',#3037,#3037,#2713,.T.);
#3562=EDGE_CURVE('',#3037,#3038,#1834,.T.);
#3563=EDGE_CURVE('',#3038,#3038,#2714,.T.);
#3564=EDGE_CURVE('',#3039,#3039,#2715,.T.);
#3565=EDGE_CURVE('',#3039,#3040,#1835,.T.);
#3566=EDGE_CURVE('',#3040,#3040,#2716,.T.);
#3567=EDGE_CURVE('',#3041,#3041,#2717,.T.);
#3568=EDGE_CURVE('',#3041,#3042,#1836,.T.);
#3569=EDGE_CURVE('',#3042,#3042,#2718,.T.);
#3570=EDGE_CURVE('',#3043,#3043,#2719,.T.);
#3571=EDGE_CURVE('',#3043,#3044,#1837,.T.);
#3572=EDGE_CURVE('',#3044,#3044,#2720,.T.);
#3573=EDGE_CURVE('',#3045,#3045,#2721,.T.);
#3574=EDGE_CURVE('',#3045,#3046,#1838,.T.);
#3575=EDGE_CURVE('',#3046,#3046,#2722,.T.);
#3576=EDGE_CURVE('',#3047,#3048,#1839,.T.);
#3577=EDGE_CURVE('',#3049,#3047,#1840,.T.);
#3578=EDGE_CURVE('',#3050,#3049,#1841,.T.);
#3579=EDGE_CURVE('',#3050,#3048,#1842,.T.);
#3580=EDGE_CURVE('',#3048,#3051,#1843,.T.);
#3581=EDGE_CURVE('',#3052,#3050,#1844,.T.);
#3582=EDGE_CURVE('',#3052,#3051,#1845,.T.);
#3583=EDGE_CURVE('',#3051,#3053,#1846,.T.);
#3584=EDGE_CURVE('',#3054,#3052,#1847,.T.);
#3585=EDGE_CURVE('',#3054,#3053,#1848,.T.);
#3586=EDGE_CURVE('',#3053,#3047,#1849,.T.);
#3587=EDGE_CURVE('',#3049,#3054,#1850,.T.);
#3588=EDGE_CURVE('',#3055,#3056,#1851,.T.);
#3589=EDGE_CURVE('',#3056,#3057,#1852,.T.);
#3590=EDGE_CURVE('',#3058,#3057,#1853,.T.);
#3591=EDGE_CURVE('',#3055,#3058,#1854,.T.);
#3592=EDGE_CURVE('',#3059,#3055,#1855,.T.);
#3593=EDGE_CURVE('',#3060,#3058,#1856,.T.);
#3594=EDGE_CURVE('',#3059,#3060,#1857,.T.);
#3595=EDGE_CURVE('',#3061,#3059,#1858,.T.);
#3596=EDGE_CURVE('',#3062,#3060,#1859,.T.);
#3597=EDGE_CURVE('',#3061,#3062,#1860,.T.);
#3598=EDGE_CURVE('',#3056,#3061,#1861,.T.);
#3599=EDGE_CURVE('',#3057,#3062,#1862,.T.);
#3600=EDGE_CURVE('',#3063,#3064,#1863,.T.);
#3601=EDGE_CURVE('',#3064,#3065,#1864,.T.);
#3602=EDGE_CURVE('',#3066,#3065,#1865,.T.);
#3603=EDGE_CURVE('',#3063,#3066,#1866,.T.);
#3604=EDGE_CURVE('',#3067,#3063,#1867,.T.);
#3605=EDGE_CURVE('',#3068,#3066,#1868,.T.);
#3606=EDGE_CURVE('',#3067,#3068,#1869,.T.);
#3607=EDGE_CURVE('',#3069,#3067,#1870,.T.);
#3608=EDGE_CURVE('',#3070,#3068,#1871,.T.);
#3609=EDGE_CURVE('',#3069,#3070,#1872,.T.);
#3610=EDGE_CURVE('',#3064,#3069,#1873,.T.);
#3611=EDGE_CURVE('',#3065,#3070,#1874,.T.);
#3612=EDGE_CURVE('',#3071,#3072,#1875,.T.);
#3613=EDGE_CURVE('',#3072,#3073,#1876,.T.);
#3614=EDGE_CURVE('',#3074,#3073,#1877,.T.);
#3615=EDGE_CURVE('',#3071,#3074,#1878,.T.);
#3616=EDGE_CURVE('',#3075,#3071,#1879,.T.);
#3617=EDGE_CURVE('',#3076,#3074,#1880,.T.);
#3618=EDGE_CURVE('',#3075,#3076,#1881,.T.);
#3619=EDGE_CURVE('',#3077,#3075,#1882,.T.);
#3620=EDGE_CURVE('',#3078,#3076,#1883,.T.);
#3621=EDGE_CURVE('',#3077,#3078,#1884,.T.);
#3622=EDGE_CURVE('',#3072,#3077,#1885,.T.);
#3623=EDGE_CURVE('',#3073,#3078,#1886,.T.);
#3624=EDGE_CURVE('',#3079,#3079,#2723,.T.);
#3625=EDGE_CURVE('',#3079,#3080,#1887,.T.);
#3626=EDGE_CURVE('',#3080,#3080,#2724,.T.);
#3627=EDGE_CURVE('',#3081,#3081,#2725,.T.);
#3628=EDGE_CURVE('',#3081,#3082,#1888,.T.);
#3629=EDGE_CURVE('',#3082,#3082,#2726,.T.);
#3630=EDGE_CURVE('',#3083,#3083,#2727,.T.);
#3631=EDGE_CURVE('',#3083,#3084,#1889,.T.);
#3632=EDGE_CURVE('',#3084,#3084,#2728,.T.);
#3633=EDGE_CURVE('',#3085,#3085,#2729,.T.);
#3634=EDGE_CURVE('',#3085,#3086,#1890,.T.);
#3635=EDGE_CURVE('',#3086,#3086,#2730,.T.);
#3636=EDGE_CURVE('',#3087,#3087,#2731,.T.);
#3637=EDGE_CURVE('',#3087,#3088,#1891,.T.);
#3638=EDGE_CURVE('',#3088,#3088,#2732,.T.);
#3639=EDGE_CURVE('',#3089,#3089,#2733,.T.);
#3640=EDGE_CURVE('',#3089,#3090,#1892,.T.);
#3641=EDGE_CURVE('',#3090,#3090,#2734,.T.);
#3642=EDGE_CURVE('',#3091,#3091,#2735,.T.);
#3643=EDGE_CURVE('',#3091,#3092,#1893,.T.);
#3644=EDGE_CURVE('',#3092,#3092,#2736,.T.);
#3645=EDGE_CURVE('',#3093,#3094,#1894,.T.);
#3646=EDGE_CURVE('',#3095,#3093,#1895,.T.);
#3647=EDGE_CURVE('',#3095,#3096,#1896,.T.);
#3648=EDGE_CURVE('',#3094,#3096,#1897,.T.);
#3649=EDGE_CURVE('',#3097,#3098,#1898,.T.);
#3650=EDGE_CURVE('',#3099,#3097,#1899,.T.);
#3651=EDGE_CURVE('',#3100,#3099,#1900,.T.);
#3652=EDGE_CURVE('',#3098,#3100,#1901,.T.);
#3653=EDGE_CURVE('',#3100,#3101,#1902,.T.);
#3654=EDGE_CURVE('',#3102,#3099,#1903,.T.);
#3655=EDGE_CURVE('',#3101,#3102,#1904,.T.);
#3656=EDGE_CURVE('',#3103,#3095,#1905,.T.);
#3657=EDGE_CURVE('',#3103,#3104,#1906,.T.);
#3658=EDGE_CURVE('',#3096,#3104,#1907,.T.);
#3659=EDGE_CURVE('',#3093,#3105,#1908,.T.);
#3660=EDGE_CURVE('',#3106,#3105,#1909,.T.);
#3661=EDGE_CURVE('',#3098,#3106,#1910,.T.);
#3662=EDGE_CURVE('',#3101,#3103,#1911,.T.);
#3663=EDGE_CURVE('',#3094,#3107,#1912,.T.);
#3664=EDGE_CURVE('',#3105,#3107,#1913,.T.);
#3665=EDGE_CURVE('',#3097,#3108,#1914,.T.);
#3666=EDGE_CURVE('',#3107,#3108,#1915,.T.);
#3667=EDGE_CURVE('',#3104,#3102,#1916,.T.);
#3668=EDGE_CURVE('',#3108,#3106,#1917,.T.);
#3669=EDGE_CURVE('',#3109,#3109,#2737,.T.);
#3670=EDGE_CURVE('',#3109,#3110,#1918,.T.);
#3671=EDGE_CURVE('',#3110,#3110,#2738,.T.);
#3672=EDGE_CURVE('',#3111,#3111,#2739,.T.);
#3673=EDGE_CURVE('',#3111,#3112,#1919,.T.);
#3674=EDGE_CURVE('',#3112,#3112,#2740,.T.);
#3675=EDGE_CURVE('',#3113,#3113,#2741,.T.);
#3676=EDGE_CURVE('',#3113,#3114,#1920,.T.);
#3677=EDGE_CURVE('',#3114,#3114,#2742,.T.);
#3678=EDGE_CURVE('',#3115,#3115,#2743,.T.);
#3679=EDGE_CURVE('',#3115,#3116,#1921,.T.);
#3680=EDGE_CURVE('',#3116,#3116,#2744,.T.);
#3681=EDGE_CURVE('',#3117,#3117,#2745,.T.);
#3682=EDGE_CURVE('',#3117,#3118,#1922,.T.);
#3683=EDGE_CURVE('',#3118,#3118,#2746,.T.);
#3684=EDGE_CURVE('',#3119,#3119,#2747,.T.);
#3685=EDGE_CURVE('',#3119,#3120,#1923,.T.);
#3686=EDGE_CURVE('',#3120,#3120,#2748,.T.);
#3687=EDGE_CURVE('',#3121,#3121,#2749,.T.);
#3688=EDGE_CURVE('',#3121,#3122,#1924,.T.);
#3689=EDGE_CURVE('',#3122,#3122,#2750,.T.);
#3690=EDGE_CURVE('',#3123,#3123,#2751,.T.);
#3691=EDGE_CURVE('',#3123,#3124,#1925,.T.);
#3692=EDGE_CURVE('',#3124,#3124,#2752,.T.);
#3693=EDGE_CURVE('',#3125,#3125,#2753,.T.);
#3694=EDGE_CURVE('',#3125,#3126,#1926,.T.);
#3695=EDGE_CURVE('',#3126,#3126,#2754,.T.);
#3696=EDGE_CURVE('',#3127,#3127,#2755,.T.);
#3697=EDGE_CURVE('',#3127,#3128,#1927,.T.);
#3698=EDGE_CURVE('',#3128,#3128,#2756,.T.);
#3699=EDGE_CURVE('',#3129,#3129,#2757,.T.);
#3700=EDGE_CURVE('',#3129,#3130,#1928,.T.);
#3701=EDGE_CURVE('',#3130,#3130,#2758,.T.);
#3702=EDGE_CURVE('',#3131,#3131,#2759,.T.);
#3703=EDGE_CURVE('',#3131,#3132,#1929,.T.);
#3704=EDGE_CURVE('',#3132,#3132,#2760,.T.);
#3705=EDGE_CURVE('',#3133,#3133,#2761,.T.);
#3706=EDGE_CURVE('',#3134,#3134,#2762,.T.);
#3707=EDGE_CURVE('',#3134,#3133,#1930,.T.);
#3708=EDGE_CURVE('',#3135,#3135,#2763,.T.);
#3709=EDGE_CURVE('',#3135,#3136,#1931,.T.);
#3710=EDGE_CURVE('',#3136,#3136,#2764,.T.);
#3711=EDGE_CURVE('',#3137,#3137,#2765,.T.);
#3712=EDGE_CURVE('',#3137,#3138,#1932,.T.);
#3713=EDGE_CURVE('',#3138,#3138,#2766,.T.);
#3714=EDGE_CURVE('',#3139,#3139,#2767,.T.);
#3715=EDGE_CURVE('',#3139,#3140,#1933,.T.);
#3716=EDGE_CURVE('',#3140,#3140,#2768,.T.);
#3717=EDGE_CURVE('',#3141,#3141,#2769,.T.);
#3718=EDGE_CURVE('',#3141,#3142,#1934,.T.);
#3719=EDGE_CURVE('',#3142,#3142,#2770,.T.);
#3720=EDGE_CURVE('',#3143,#3143,#2771,.T.);
#3721=EDGE_CURVE('',#3143,#3144,#1935,.T.);
#3722=EDGE_CURVE('',#3144,#3144,#2772,.T.);
#3723=EDGE_CURVE('',#3145,#3145,#2773,.T.);
#3724=EDGE_CURVE('',#3145,#3146,#1936,.T.);
#3725=EDGE_CURVE('',#3146,#3146,#2774,.T.);
#3726=EDGE_CURVE('',#3147,#3147,#2775,.T.);
#3727=EDGE_CURVE('',#3147,#3148,#1937,.T.);
#3728=EDGE_CURVE('',#3148,#3148,#2776,.T.);
#3729=EDGE_CURVE('',#3149,#3149,#2777,.T.);
#3730=EDGE_CURVE('',#3149,#3150,#1938,.T.);
#3731=EDGE_CURVE('',#3150,#3150,#2778,.T.);
#3732=EDGE_CURVE('',#3151,#3152,#1939,.T.);
#3733=EDGE_CURVE('',#3153,#3151,#1940,.T.);
#3734=EDGE_CURVE('',#3153,#3154,#1941,.T.);
#3735=EDGE_CURVE('',#3152,#3154,#1942,.T.);
#3736=EDGE_CURVE('',#3155,#3156,#1943,.T.);
#3737=EDGE_CURVE('',#3157,#3155,#1944,.T.);
#3738=EDGE_CURVE('',#3158,#3157,#1945,.T.);
#3739=EDGE_CURVE('',#3156,#3158,#1946,.T.);
#3740=EDGE_CURVE('',#3158,#3159,#1947,.T.);
#3741=EDGE_CURVE('',#3160,#3157,#1948,.T.);
#3742=EDGE_CURVE('',#3159,#3160,#1949,.T.);
#3743=EDGE_CURVE('',#3161,#3153,#1950,.T.);
#3744=EDGE_CURVE('',#3161,#3162,#1951,.T.);
#3745=EDGE_CURVE('',#3154,#3162,#1952,.T.);
#3746=EDGE_CURVE('',#3151,#3163,#1953,.T.);
#3747=EDGE_CURVE('',#3164,#3163,#1954,.T.);
#3748=EDGE_CURVE('',#3156,#3164,#1955,.T.);
#3749=EDGE_CURVE('',#3159,#3161,#1956,.T.);
#3750=EDGE_CURVE('',#3152,#3165,#1957,.T.);
#3751=EDGE_CURVE('',#3163,#3165,#1958,.T.);
#3752=EDGE_CURVE('',#3155,#3166,#1959,.T.);
#3753=EDGE_CURVE('',#3165,#3166,#1960,.T.);
#3754=EDGE_CURVE('',#3162,#3160,#1961,.T.);
#3755=EDGE_CURVE('',#3166,#3164,#1962,.T.);
#3756=EDGE_CURVE('',#3167,#3167,#2779,.T.);
#3757=EDGE_CURVE('',#3167,#3168,#1963,.T.);
#3758=EDGE_CURVE('',#3168,#3168,#2780,.T.);
#3759=EDGE_CURVE('',#3169,#3169,#2781,.T.);
#3760=EDGE_CURVE('',#3169,#3170,#1964,.T.);
#3761=EDGE_CURVE('',#3170,#3170,#2782,.T.);
#3762=EDGE_CURVE('',#3171,#3171,#2783,.T.);
#3763=EDGE_CURVE('',#3171,#3172,#1965,.T.);
#3764=EDGE_CURVE('',#3172,#3172,#2784,.T.);
#3765=EDGE_CURVE('',#3173,#3173,#2785,.T.);
#3766=EDGE_CURVE('',#3173,#3174,#1966,.T.);
#3767=EDGE_CURVE('',#3174,#3174,#2786,.T.);
#3768=EDGE_CURVE('',#3175,#3175,#2787,.T.);
#3769=EDGE_CURVE('',#3175,#3176,#1967,.T.);
#3770=EDGE_CURVE('',#3176,#3176,#2788,.T.);
#3771=EDGE_CURVE('',#3177,#3177,#2789,.T.);
#3772=EDGE_CURVE('',#3177,#3178,#1968,.T.);
#3773=EDGE_CURVE('',#3178,#3178,#2790,.T.);
#3774=EDGE_CURVE('',#3179,#3179,#2791,.T.);
#3775=EDGE_CURVE('',#3179,#3180,#1969,.T.);
#3776=EDGE_CURVE('',#3180,#3180,#2792,.T.);
#3777=EDGE_CURVE('',#3181,#3181,#2793,.T.);
#3778=EDGE_CURVE('',#3181,#3182,#1970,.T.);
#3779=EDGE_CURVE('',#3182,#3182,#2794,.T.);
#3780=EDGE_CURVE('',#3183,#3183,#2795,.T.);
#3781=EDGE_CURVE('',#3183,#3184,#1971,.T.);
#3782=EDGE_CURVE('',#3184,#3184,#2796,.T.);
#3783=EDGE_CURVE('',#3185,#3185,#2797,.T.);
#3784=EDGE_CURVE('',#3185,#3186,#1972,.T.);
#3785=EDGE_CURVE('',#3186,#3186,#2798,.T.);
#3786=EDGE_CURVE('',#3187,#3187,#2799,.T.);
#3787=EDGE_CURVE('',#3187,#3188,#1973,.T.);
#3788=EDGE_CURVE('',#3188,#3188,#2800,.T.);
#3789=EDGE_CURVE('',#3189,#3189,#2801,.T.);
#3790=EDGE_CURVE('',#3189,#3190,#1974,.T.);
#3791=EDGE_CURVE('',#3190,#3190,#2802,.T.);
#3792=EDGE_CURVE('',#3191,#3191,#2803,.T.);
#3793=EDGE_CURVE('',#3192,#3192,#2804,.T.);
#3794=EDGE_CURVE('',#3192,#3191,#1975,.T.);
#3795=EDGE_CURVE('',#3193,#3193,#2805,.T.);
#3796=EDGE_CURVE('',#3193,#3194,#1976,.T.);
#3797=EDGE_CURVE('',#3194,#3194,#2806,.T.);
#3798=EDGE_CURVE('',#3195,#3195,#2807,.T.);
#3799=EDGE_CURVE('',#3195,#3196,#1977,.T.);
#3800=EDGE_CURVE('',#3196,#3196,#2808,.T.);
#3801=EDGE_CURVE('',#3197,#3197,#2809,.T.);
#3802=EDGE_CURVE('',#3197,#3198,#1978,.T.);
#3803=EDGE_CURVE('',#3198,#3198,#2810,.T.);
#3804=EDGE_CURVE('',#3199,#3199,#2811,.T.);
#3805=EDGE_CURVE('',#3199,#3200,#1979,.T.);
#3806=EDGE_CURVE('',#3200,#3200,#2812,.T.);
#3807=EDGE_CURVE('',#3201,#3201,#2813,.T.);
#3808=EDGE_CURVE('',#3201,#3202,#1980,.T.);
#3809=EDGE_CURVE('',#3202,#3202,#2814,.T.);
#3810=EDGE_CURVE('',#3203,#3203,#2815,.T.);
#3811=EDGE_CURVE('',#3203,#3204,#1981,.T.);
#3812=EDGE_CURVE('',#3204,#3204,#2816,.T.);
#3813=EDGE_CURVE('',#3205,#3205,#2817,.T.);
#3814=EDGE_CURVE('',#3206,#3206,#2818,.T.);
#3815=EDGE_CURVE('',#3206,#3205,#1982,.T.);
#3816=EDGE_CURVE('',#3207,#3207,#2819,.T.);
#3817=EDGE_CURVE('',#3207,#3208,#1983,.T.);
#3818=EDGE_CURVE('',#3208,#3208,#2820,.T.);
#3819=EDGE_CURVE('',#3209,#3209,#2821,.T.);
#3820=EDGE_CURVE('',#3210,#3210,#2822,.T.);
#3821=EDGE_CURVE('',#3210,#3209,#1984,.T.);
#3822=EDGE_CURVE('',#3211,#3211,#2823,.T.);
#3823=EDGE_CURVE('',#3211,#3212,#1985,.T.);
#3824=EDGE_CURVE('',#3212,#3212,#2824,.T.);
#3825=EDGE_CURVE('',#3213,#3213,#2825,.T.);
#3826=EDGE_CURVE('',#3214,#3214,#2826,.T.);
#3827=EDGE_CURVE('',#3214,#3213,#1986,.T.);
#3828=EDGE_CURVE('',#3215,#3216,#1987,.T.);
#3829=EDGE_CURVE('',#3215,#3217,#1988,.T.);
#3830=EDGE_CURVE('',#3218,#3217,#1989,.T.);
#3831=EDGE_CURVE('',#3219,#3218,#1990,.T.);
#3832=EDGE_CURVE('',#3220,#3219,#1991,.T.);
#3833=EDGE_CURVE('',#3221,#3220,#1992,.T.);
#3834=EDGE_CURVE('',#3222,#3221,#1993,.T.);
#3835=EDGE_CURVE('',#3223,#3222,#1994,.T.);
#3836=EDGE_CURVE('',#3224,#3223,#1995,.T.);
#3837=EDGE_CURVE('',#3224,#3225,#1996,.T.);
#3838=EDGE_CURVE('',#3226,#3225,#1997,.T.);
#3839=EDGE_CURVE('',#3216,#3226,#1998,.T.);
#3840=EDGE_CURVE('',#3227,#3228,#1999,.T.);
#3841=EDGE_CURVE('',#3228,#3218,#2000,.T.);
#3842=EDGE_CURVE('',#3217,#3227,#2001,.T.);
#3843=EDGE_CURVE('',#3229,#3230,#2002,.T.);
#3844=EDGE_CURVE('',#3230,#3224,#2003,.T.);
#3845=EDGE_CURVE('',#3223,#3229,#2004,.T.);
#3846=EDGE_CURVE('',#3231,#3220,#2005,.T.);
#3847=EDGE_CURVE('',#3232,#3231,#2006,.T.);
#3848=EDGE_CURVE('',#3221,#3232,#2007,.T.);
#3849=EDGE_CURVE('',#3219,#3233,#2008,.T.);
#3850=EDGE_CURVE('',#3233,#3231,#2009,.T.);
#3851=EDGE_CURVE('',#3232,#3234,#2010,.T.);
#3852=EDGE_CURVE('',#3234,#3233,#2011,.T.);
#3853=EDGE_CURVE('',#3234,#3222,#2012,.T.);
#3854=EDGE_CURVE('',#3229,#3228,#2013,.T.);
#3855=EDGE_CURVE('',#3235,#3226,#2014,.T.);
#3856=EDGE_CURVE('',#3235,#3236,#2015,.T.);
#3857=EDGE_CURVE('',#3236,#3216,#2016,.T.);
#3858=EDGE_CURVE('',#3237,#3225,#2017,.T.);
#3859=EDGE_CURVE('',#3237,#3235,#2018,.T.);
#3860=EDGE_CURVE('',#3236,#3238,#2019,.T.);
#3861=EDGE_CURVE('',#3238,#3215,#2020,.T.);
#3862=EDGE_CURVE('',#3238,#3237,#2021,.T.);
#3863=EDGE_CURVE('',#3230,#3227,#2022,.T.);
#3864=EDGE_CURVE('',#3239,#3239,#2827,.T.);
#3865=EDGE_CURVE('',#3239,#3240,#2023,.T.);
#3866=EDGE_CURVE('',#3240,#3240,#2828,.T.);
#3867=EDGE_CURVE('',#3241,#3241,#2829,.T.);
#3868=EDGE_CURVE('',#3241,#3242,#2024,.T.);
#3869=EDGE_CURVE('',#3242,#3242,#2830,.T.);
#3870=EDGE_CURVE('',#3243,#3243,#2831,.T.);
#3871=EDGE_CURVE('',#3243,#3244,#2025,.T.);
#3872=EDGE_CURVE('',#3244,#3244,#2832,.T.);
#3873=EDGE_CURVE('',#3245,#3245,#2833,.T.);
#3874=EDGE_CURVE('',#3245,#3246,#2026,.T.);
#3875=EDGE_CURVE('',#3246,#3246,#2834,.T.);
#3876=EDGE_CURVE('',#3247,#3247,#2835,.T.);
#3877=EDGE_CURVE('',#3247,#3248,#2027,.T.);
#3878=EDGE_CURVE('',#3248,#3248,#2836,.T.);
#3879=EDGE_CURVE('',#3249,#3249,#2837,.T.);
#3880=EDGE_CURVE('',#3249,#3250,#2028,.T.);
#3881=EDGE_CURVE('',#3250,#3250,#2838,.T.);
#3882=EDGE_CURVE('',#3251,#3251,#2839,.T.);
#3883=EDGE_CURVE('',#3251,#3252,#2029,.T.);
#3884=EDGE_CURVE('',#3252,#3252,#2840,.T.);
#3885=EDGE_CURVE('',#3253,#3253,#2841,.T.);
#3886=EDGE_CURVE('',#3254,#3254,#2842,.T.);
#3887=EDGE_CURVE('',#3254,#3253,#2030,.T.);
#3888=EDGE_CURVE('',#3255,#3255,#2843,.T.);
#3889=EDGE_CURVE('',#3255,#3256,#2031,.T.);
#3890=EDGE_CURVE('',#3256,#3256,#2844,.T.);
#3891=EDGE_CURVE('',#3257,#3257,#2845,.T.);
#3892=EDGE_CURVE('',#3257,#3258,#332,.T.);
#3893=EDGE_CURVE('',#3258,#3258,#2846,.T.);
#3894=EDGE_CURVE('',#3259,#3260,#2847,.T.);
#3895=EDGE_CURVE('',#3260,#3259,#2848,.T.);
#3896=EDGE_CURVE('',#3260,#3261,#2849,.T.);
#3897=EDGE_CURVE('',#3262,#3261,#2850,.T.);
#3898=EDGE_CURVE('',#3261,#3262,#2851,.T.);
#3899=EDGE_CURVE('',#3262,#3263,#2032,.T.);
#3900=EDGE_CURVE('',#3263,#3263,#2852,.T.);
#3901=EDGE_CURVE('',#3264,#3264,#2853,.T.);
#3902=EDGE_CURVE('',#3264,#3265,#2033,.T.);
#3903=EDGE_CURVE('',#3265,#3265,#2854,.T.);
#3904=EDGE_CURVE('',#3265,#3266,#2034,.T.);
#3905=EDGE_CURVE('',#3266,#3266,#2855,.T.);
#3906=EDGE_CURVE('',#3267,#3267,#2856,.T.);
#3907=EDGE_CURVE('',#3267,#3259,#2035,.T.);
#3908=EDGE_CURVE('',#3268,#3268,#2857,.T.);
#3909=EDGE_CURVE('',#3268,#3264,#2036,.T.);
#3910=EDGE_CURVE('',#3269,#3270,#2858,.T.);
#3911=EDGE_CURVE('',#3270,#3269,#2859,.T.);
#3912=EDGE_CURVE('',#3270,#3271,#2860,.T.);
#3913=EDGE_CURVE('',#3272,#3271,#2861,.T.);
#3914=EDGE_CURVE('',#3271,#3272,#2862,.T.);
#3915=EDGE_CURVE('',#3273,#3273,#2863,.T.);
#3916=EDGE_CURVE('',#3273,#3272,#2037,.T.);
#3917=EDGE_CURVE('',#3274,#3274,#2864,.T.);
#3918=EDGE_CURVE('',#3275,#3275,#2865,.T.);
#3919=EDGE_CURVE('',#3276,#3276,#2866,.T.);
#3920=EDGE_CURVE('',#3276,#3274,#2038,.T.);
#3921=EDGE_CURVE('',#3277,#3277,#2867,.T.);
#3922=EDGE_CURVE('',#3277,#3276,#2039,.T.);
#3923=EDGE_CURVE('',#3278,#3278,#2868,.T.);
#3924=EDGE_CURVE('',#3278,#3277,#2040,.T.);
#3925=EDGE_CURVE('',#3269,#3275,#2041,.T.);
#3926=EDGE_CURVE('',#3279,#3280,#2869,.T.);
#3927=EDGE_CURVE('',#3281,#3282,#2870,.T.);
#3928=EDGE_CURVE('',#3283,#3284,#2871,.T.);
#3929=EDGE_CURVE('',#3285,#3286,#2872,.T.);
#3930=EDGE_CURVE('',#3287,#3288,#2873,.T.);
#3931=EDGE_CURVE('',#3289,#3290,#2874,.T.);
#3932=EDGE_CURVE('',#3291,#3292,#2875,.T.);
#3933=EDGE_CURVE('',#3293,#3294,#333,.T.);
#3934=EDGE_CURVE('',#3295,#3293,#2876,.T.);
#3935=EDGE_CURVE('',#3296,#3295,#334,.T.);
#3936=EDGE_CURVE('',#3294,#3296,#2877,.T.);
#3937=EDGE_CURVE('',#3297,#3295,#2878,.T.);
#3938=EDGE_CURVE('',#3297,#3298,#335,.T.);
#3939=EDGE_CURVE('',#3299,#3298,#2879,.T.);
#3940=EDGE_CURVE('',#3299,#3300,#336,.T.);
#3941=EDGE_CURVE('',#3301,#3300,#2880,.T.);
#3942=EDGE_CURVE('',#3301,#3302,#2042,.T.);
#3943=EDGE_CURVE('',#3302,#3302,#2881,.T.);
#3944=EDGE_CURVE('',#3303,#3301,#2882,.T.);
#3945=EDGE_CURVE('',#3303,#3304,#337,.T.);
#3946=EDGE_CURVE('',#3305,#3304,#2883,.T.);
#3947=EDGE_CURVE('',#3305,#3306,#338,.T.);
#3948=EDGE_CURVE('',#3307,#3306,#2884,.T.);
#3949=EDGE_CURVE('',#3307,#3308,#339,.T.);
#3950=EDGE_CURVE('',#3309,#3308,#2885,.T.);
#3951=EDGE_CURVE('',#3309,#3310,#340,.T.);
#3952=EDGE_CURVE('',#3296,#3310,#2886,.T.);
#3953=EDGE_CURVE('',#3293,#3311,#2887,.T.);
#3954=EDGE_CURVE('',#3311,#3297,#2888,.T.);
#3955=EDGE_CURVE('',#3312,#3311,#341,.T.);
#3956=EDGE_CURVE('',#3298,#3312,#2889,.T.);
#3957=EDGE_CURVE('',#3312,#3313,#2890,.T.);
#3958=EDGE_CURVE('',#3313,#3299,#2891,.T.);
#3959=EDGE_CURVE('',#3314,#3313,#342,.T.);
#3960=EDGE_CURVE('',#3300,#3314,#2892,.T.);
#3961=EDGE_CURVE('',#3314,#3315,#2893,.T.);
#3962=EDGE_CURVE('',#3315,#3316,#2894,.T.);
#3963=EDGE_CURVE('',#3316,#3303,#2895,.T.);
#3964=EDGE_CURVE('',#3317,#3316,#343,.T.);
#3965=EDGE_CURVE('',#3304,#3317,#2896,.T.);
#3966=EDGE_CURVE('',#3317,#3318,#2897,.T.);
#3967=EDGE_CURVE('',#3318,#3305,#2898,.T.);
#3968=EDGE_CURVE('',#3319,#3318,#344,.T.);
#3969=EDGE_CURVE('',#3306,#3319,#2899,.T.);
#3970=EDGE_CURVE('',#3319,#3320,#2900,.T.);
#3971=EDGE_CURVE('',#3320,#3307,#2901,.T.);
#3972=EDGE_CURVE('',#3321,#3320,#345,.T.);
#3973=EDGE_CURVE('',#3308,#3321,#2902,.T.);
#3974=EDGE_CURVE('',#3322,#3322,#2903,.T.);
#3975=EDGE_CURVE('',#3322,#3315,#2043,.T.);
#3976=EDGE_CURVE('',#3323,#3294,#2904,.T.);
#3977=EDGE_CURVE('',#3323,#3324,#346,.T.);
#3978=EDGE_CURVE('',#3321,#3324,#2905,.T.);
#3979=EDGE_CURVE('',#3310,#3323,#2906,.T.);
#3980=EDGE_CURVE('',#3324,#3309,#2907,.T.);
#3981=EDGE_CURVE('',#3325,#3325,#2908,.T.);
#3982=EDGE_CURVE('',#3326,#3326,#2909,.T.);
#3983=EDGE_CURVE('',#3327,#3327,#2910,.T.);
#3984=EDGE_CURVE('',#3327,#3325,#2044,.T.);
#3985=EDGE_CURVE('',#3328,#3328,#2911,.T.);
#3986=EDGE_CURVE('',#3328,#3326,#2045,.T.);
#3987=EDGE_CURVE('',#3329,#3329,#2912,.T.);
#3988=EDGE_CURVE('',#3330,#3330,#2913,.T.);
#3989=EDGE_CURVE('',#3331,#3331,#2914,.T.);
#3990=EDGE_CURVE('',#3331,#3329,#2046,.T.);
#3991=EDGE_CURVE('',#3332,#3332,#2915,.T.);
#3992=EDGE_CURVE('',#3332,#3330,#2047,.T.);
#3993=EDGE_CURVE('',#3333,#3333,#2916,.T.);
#3994=EDGE_CURVE('',#3334,#3334,#2917,.T.);
#3995=EDGE_CURVE('',#3334,#3333,#2048,.T.);
#3996=EDGE_CURVE('',#3335,#3335,#2918,.T.);
#3997=EDGE_CURVE('',#3335,#3334,#2049,.T.);
#3998=EDGE_CURVE('',#3336,#3336,#2919,.T.);
#3999=EDGE_CURVE('',#3336,#3335,#2050,.T.);
#4000=EDGE_CURVE('',#3337,#3337,#2920,.T.);
#4001=EDGE_CURVE('',#3338,#3338,#2921,.F.);
#4002=EDGE_CURVE('',#3338,#3337,#2051,.T.);
#4003=EDGE_CURVE('',#3339,#3339,#2922,.F.);
#4004=EDGE_CURVE('',#3339,#3338,#2052,.T.);
#4005=EDGE_CURVE('',#3340,#3340,#2923,.T.);
#4006=EDGE_CURVE('',#3340,#3339,#2053,.T.);
#4007=EDGE_CURVE('',#3341,#3342,#2054,.T.);
#4008=EDGE_CURVE('',#3342,#3343,#2055,.T.);
#4009=EDGE_CURVE('',#3343,#3344,#2056,.T.);
#4010=EDGE_CURVE('',#3341,#3344,#2057,.T.);
#4011=EDGE_CURVE('',#3342,#3345,#2058,.T.);
#4012=EDGE_CURVE('',#3345,#3346,#2059,.T.);
#4013=EDGE_CURVE('',#3346,#3343,#2060,.T.);
#4014=EDGE_CURVE('',#3345,#3347,#2061,.T.);
#4015=EDGE_CURVE('',#3347,#3348,#2062,.T.);
#4016=EDGE_CURVE('',#3348,#3346,#2063,.T.);
#4017=EDGE_CURVE('',#3347,#3349,#2064,.T.);
#4018=EDGE_CURVE('',#3349,#3350,#2065,.T.);
#4019=EDGE_CURVE('',#3350,#3348,#2066,.T.);
#4020=EDGE_CURVE('',#3349,#3351,#2067,.T.);
#4021=EDGE_CURVE('',#3351,#3352,#2068,.T.);
#4022=EDGE_CURVE('',#3352,#3350,#2069,.T.);
#4023=EDGE_CURVE('',#3351,#3341,#2070,.T.);
#4024=EDGE_CURVE('',#3344,#3352,#2071,.T.);
#4025=EDGE_CURVE('',#3353,#3354,#2924,.T.);
#4026=EDGE_CURVE('',#3355,#3353,#2072,.T.);
#4027=EDGE_CURVE('',#3356,#3355,#2073,.T.);
#4028=EDGE_CURVE('',#3354,#3356,#2074,.T.);
#4029=EDGE_CURVE('',#3354,#3357,#2075,.T.);
#4030=EDGE_CURVE('',#3358,#3356,#2076,.T.);
#4031=EDGE_CURVE('',#3358,#3357,#2077,.T.);
#4032=EDGE_CURVE('',#3357,#3359,#2925,.T.);
#4033=EDGE_CURVE('',#3360,#3358,#2078,.T.);
#4034=EDGE_CURVE('',#3359,#3360,#2079,.T.);
#4035=EDGE_CURVE('',#3359,#3353,#2080,.T.);
#4036=EDGE_CURVE('',#3360,#3355,#2081,.T.);
#4037=EDGE_CURVE('',#3361,#3361,#2926,.T.);
#4038=EDGE_CURVE('',#3362,#3362,#2927,.T.);
#4039=EDGE_CURVE('',#3363,#3363,#2928,.T.);
#4040=EDGE_CURVE('',#3363,#3361,#2082,.T.);
#4041=EDGE_CURVE('',#3364,#3364,#2929,.T.);
#4042=EDGE_CURVE('',#3365,#3365,#2930,.T.);
#4043=EDGE_CURVE('',#3365,#3364,#2083,.T.);
#4044=EDGE_CURVE('',#3366,#3366,#2931,.T.);
#4045=EDGE_CURVE('',#3367,#3367,#2932,.T.);
#4046=EDGE_CURVE('',#3367,#3366,#2084,.T.);
#4047=EDGE_CURVE('',#3368,#3368,#2933,.T.);
#4048=EDGE_CURVE('',#3369,#3369,#2934,.T.);
#4049=EDGE_CURVE('',#3369,#3368,#2085,.T.);
#4050=EDGE_CURVE('',#3370,#3370,#2935,.T.);
#4051=EDGE_CURVE('',#3371,#3371,#2936,.T.);
#4052=EDGE_CURVE('',#3371,#3370,#2086,.T.);
#4053=EDGE_CURVE('',#3372,#3372,#2937,.T.);
#4054=EDGE_CURVE('',#3372,#3362,#2087,.T.);
#4055=EDGE_CURVE('',#3373,#3374,#2938,.T.);
#4056=EDGE_CURVE('',#3375,#3373,#2088,.T.);
#4057=EDGE_CURVE('',#3376,#3375,#2939,.T.);
#4058=EDGE_CURVE('',#3374,#3376,#2089,.T.);
#4059=EDGE_CURVE('',#3374,#3377,#2090,.T.);
#4060=EDGE_CURVE('',#3378,#3376,#2091,.T.);
#4061=EDGE_CURVE('',#3378,#3377,#2092,.T.);
#4062=EDGE_CURVE('',#3377,#3379,#2940,.T.);
#4063=EDGE_CURVE('',#3380,#3378,#2941,.T.);
#4064=EDGE_CURVE('',#3379,#3380,#2093,.T.);
#4065=EDGE_CURVE('',#3379,#3373,#2094,.T.);
#4066=EDGE_CURVE('',#3375,#3380,#2095,.T.);
#4067=EDGE_CURVE('',#3381,#3381,#2942,.T.);
#4068=EDGE_CURVE('',#3382,#3382,#2943,.T.);
#4069=EDGE_CURVE('',#3383,#3383,#2944,.T.);
#4070=EDGE_CURVE('',#3383,#3381,#2096,.T.);
#4071=EDGE_CURVE('',#3384,#3384,#2945,.T.);
#4072=EDGE_CURVE('',#3384,#3382,#2097,.T.);
#4073=EDGE_CURVE('',#3385,#3386,#2098,.T.);
#4074=EDGE_CURVE('',#3386,#3387,#2099,.T.);
#4075=EDGE_CURVE('',#3387,#3388,#2100,.T.);
#4076=EDGE_CURVE('',#3385,#3388,#2101,.T.);
#4077=EDGE_CURVE('',#3386,#3389,#2102,.T.);
#4078=EDGE_CURVE('',#3389,#3390,#2103,.T.);
#4079=EDGE_CURVE('',#3390,#3387,#2104,.T.);
#4080=EDGE_CURVE('',#3389,#3391,#2105,.T.);
#4081=EDGE_CURVE('',#3391,#3392,#2106,.T.);
#4082=EDGE_CURVE('',#3392,#3390,#2107,.T.);
#4083=EDGE_CURVE('',#3391,#3393,#2108,.T.);
#4084=EDGE_CURVE('',#3393,#3394,#2109,.T.);
#4085=EDGE_CURVE('',#3394,#3392,#2110,.T.);
#4086=EDGE_CURVE('',#3393,#3395,#2111,.T.);
#4087=EDGE_CURVE('',#3395,#3396,#2112,.T.);
#4088=EDGE_CURVE('',#3396,#3394,#2113,.T.);
#4089=EDGE_CURVE('',#3395,#3385,#2114,.T.);
#4090=EDGE_CURVE('',#3388,#3396,#2115,.T.);
#4091=EDGE_CURVE('',#3397,#3397,#2946,.T.);
#4092=EDGE_CURVE('',#3398,#3398,#2947,.T.);
#4093=EDGE_CURVE('',#3399,#3399,#2948,.T.);
#4094=EDGE_CURVE('',#3399,#3398,#2116,.T.);
#4095=EDGE_CURVE('',#3400,#3400,#2949,.T.);
#4096=EDGE_CURVE('',#3400,#3399,#2117,.T.);
#4097=EDGE_CURVE('',#3401,#3401,#2950,.T.);
#4098=EDGE_CURVE('',#3401,#3400,#2118,.T.);
#4099=EDGE_CURVE('',#3402,#3402,#2951,.T.);
#4100=EDGE_CURVE('',#3403,#3403,#2952,.F.);
#4101=EDGE_CURVE('',#3403,#3402,#2119,.T.);
#4102=EDGE_CURVE('',#3397,#3403,#2120,.T.);
#4103=EDGE_CURVE('',#3404,#3404,#2953,.T.);
#4104=EDGE_CURVE('',#3404,#3405,#2121,.T.);
#4105=EDGE_CURVE('',#3405,#3405,#2954,.T.);
#4106=EDGE_CURVE('',#3406,#3406,#2955,.T.);
#4107=EDGE_CURVE('',#3406,#3407,#2122,.T.);
#4108=EDGE_CURVE('',#3407,#3407,#2956,.T.);
#4109=EDGE_CURVE('',#3408,#3409,#2123,.T.);
#4110=EDGE_CURVE('',#3408,#3410,#2124,.T.);
#4111=EDGE_CURVE('',#3411,#3410,#2125,.T.);
#4112=EDGE_CURVE('',#3411,#3409,#2126,.T.);
#4113=EDGE_CURVE('',#3409,#3412,#2957,.T.);
#4114=EDGE_CURVE('',#3413,#3411,#2127,.T.);
#4115=EDGE_CURVE('',#3412,#3413,#2128,.T.);
#4116=EDGE_CURVE('',#3412,#3414,#2129,.T.);
#4117=EDGE_CURVE('',#3413,#3415,#2130,.T.);
#4118=EDGE_CURVE('',#3415,#3414,#2131,.T.);
#4119=EDGE_CURVE('',#3410,#3415,#2132,.T.);
#4120=EDGE_CURVE('',#3414,#3408,#2958,.T.);
#4121=EDGE_CURVE('',#3416,#3417,#2133,.T.);
#4122=EDGE_CURVE('',#3416,#3418,#2134,.T.);
#4123=EDGE_CURVE('',#3419,#3418,#2135,.T.);
#4124=EDGE_CURVE('',#3419,#3417,#2136,.T.);
#4125=EDGE_CURVE('',#3417,#3420,#2959,.T.);
#4126=EDGE_CURVE('',#3421,#3419,#2137,.T.);
#4127=EDGE_CURVE('',#3420,#3421,#2138,.T.);
#4128=EDGE_CURVE('',#3420,#3422,#2139,.T.);
#4129=EDGE_CURVE('',#3421,#3423,#2140,.T.);
#4130=EDGE_CURVE('',#3423,#3422,#2141,.T.);
#4131=EDGE_CURVE('',#3418,#3423,#2142,.T.);
#4132=EDGE_CURVE('',#3422,#3416,#2960,.T.);
#4133=EDGE_CURVE('',#3424,#3424,#2961,.T.);
#4134=EDGE_CURVE('',#3424,#3425,#2143,.T.);
#4135=EDGE_CURVE('',#3425,#3425,#2962,.T.);
#4136=EDGE_CURVE('',#3426,#3426,#2963,.T.);
#4137=EDGE_CURVE('',#3426,#3427,#2144,.T.);
#4138=EDGE_CURVE('',#3427,#3427,#2964,.T.);
#4139=EDGE_CURVE('',#3428,#3428,#2965,.T.);
#4140=EDGE_CURVE('',#3428,#3429,#2145,.T.);
#4141=EDGE_CURVE('',#3429,#3429,#2966,.T.);
#4142=EDGE_CURVE('',#3430,#3430,#2967,.T.);
#4143=EDGE_CURVE('',#3430,#3431,#2146,.T.);
#4144=EDGE_CURVE('',#3431,#3431,#2968,.T.);
#4145=EDGE_CURVE('',#3432,#3432,#2969,.T.);
#4146=EDGE_CURVE('',#3432,#3433,#2147,.T.);
#4147=EDGE_CURVE('',#3433,#3433,#2970,.T.);
#4148=EDGE_CURVE('',#3434,#3434,#2971,.T.);
#4149=EDGE_CURVE('',#3434,#3435,#2148,.T.);
#4150=EDGE_CURVE('',#3435,#3435,#2972,.T.);
#4151=EDGE_CURVE('',#3436,#3436,#2973,.T.);
#4152=EDGE_CURVE('',#3436,#3437,#2149,.T.);
#4153=EDGE_CURVE('',#3437,#3437,#2974,.T.);
#4154=EDGE_CURVE('',#3438,#3438,#2975,.T.);
#4155=EDGE_CURVE('',#3438,#3439,#2150,.T.);
#4156=EDGE_CURVE('',#3439,#3439,#2976,.T.);
#4157=EDGE_CURVE('',#3440,#3440,#2977,.T.);
#4158=EDGE_CURVE('',#3440,#3441,#2151,.T.);
#4159=EDGE_CURVE('',#3441,#3441,#2978,.T.);
#4160=EDGE_CURVE('',#3442,#3443,#2152,.T.);
#4161=EDGE_CURVE('',#3442,#3444,#2153,.T.);
#4162=EDGE_CURVE('',#3445,#3444,#2154,.T.);
#4163=EDGE_CURVE('',#3443,#3445,#2155,.T.);
#4164=EDGE_CURVE('',#3446,#3442,#2156,.T.);
#4165=EDGE_CURVE('',#3446,#3447,#2157,.T.);
#4166=EDGE_CURVE('',#3444,#3447,#2158,.T.);
#4167=EDGE_CURVE('',#3448,#3446,#2159,.T.);
#4168=EDGE_CURVE('',#3449,#3448,#2160,.T.);
#4169=EDGE_CURVE('',#3447,#3449,#2161,.T.);
#4170=EDGE_CURVE('',#3450,#3450,#2979,.T.);
#4171=EDGE_CURVE('',#3449,#3445,#2980,.T.);
#4172=EDGE_CURVE('',#3443,#3448,#2981,.T.);
#4173=EDGE_CURVE('',#3451,#3451,#2982,.T.);
#4174=EDGE_CURVE('',#3451,#3452,#2162,.T.);
#4175=EDGE_CURVE('',#3452,#3452,#2983,.T.);
#4176=EDGE_CURVE('',#3450,#3453,#2163,.T.);
#4177=EDGE_CURVE('',#3453,#3453,#2984,.T.);
#4178=EDGE_CURVE('',#3454,#3454,#2985,.T.);
#4179=EDGE_CURVE('',#3454,#3455,#2164,.T.);
#4180=EDGE_CURVE('',#3455,#3455,#2986,.T.);
#4181=EDGE_CURVE('',#3456,#3456,#2987,.T.);
#4182=EDGE_CURVE('',#3456,#3457,#2165,.T.);
#4183=EDGE_CURVE('',#3457,#3457,#2988,.T.);
#4184=EDGE_CURVE('',#3458,#3459,#2166,.T.);
#4185=EDGE_CURVE('',#3458,#3460,#2167,.T.);
#4186=EDGE_CURVE('',#3461,#3460,#2168,.T.);
#4187=EDGE_CURVE('',#3459,#3461,#2169,.T.);
#4188=EDGE_CURVE('',#3462,#3458,#2170,.T.);
#4189=EDGE_CURVE('',#3462,#3463,#2171,.T.);
#4190=EDGE_CURVE('',#3460,#3463,#2172,.T.);
#4191=EDGE_CURVE('',#3464,#3462,#2173,.T.);
#4192=EDGE_CURVE('',#3465,#3464,#2174,.T.);
#4193=EDGE_CURVE('',#3463,#3465,#2175,.T.);
#4194=EDGE_CURVE('',#3466,#3466,#2989,.T.);
#4195=EDGE_CURVE('',#3465,#3461,#2990,.T.);
#4196=EDGE_CURVE('',#3464,#3459,#2991,.T.);
#4197=EDGE_CURVE('',#3467,#3468,#2176,.T.);
#4198=EDGE_CURVE('',#3469,#3467,#2992,.T.);
#4199=EDGE_CURVE('',#3470,#3469,#2177,.T.);
#4200=EDGE_CURVE('',#3470,#3468,#2993,.T.);
#4201=EDGE_CURVE('',#3470,#3471,#2178,.T.);
#4202=EDGE_CURVE('',#3472,#3471,#2994,.T.);
#4203=EDGE_CURVE('',#3472,#3468,#2179,.T.);
#4204=EDGE_CURVE('',#3473,#3469,#2180,.T.);
#4205=EDGE_CURVE('',#3471,#3473,#2181,.T.);
#4206=EDGE_CURVE('',#3474,#3472,#2182,.T.);
#4207=EDGE_CURVE('',#3467,#3474,#2183,.T.);
#4208=EDGE_CURVE('',#3473,#3474,#2995,.T.);
#4209=EDGE_CURVE('',#3466,#3475,#2184,.T.);
#4210=EDGE_CURVE('',#3475,#3475,#2996,.T.);
#4211=EDGE_CURVE('',#3476,#3476,#2997,.T.);
#4212=EDGE_CURVE('',#3476,#3477,#2185,.T.);
#4213=EDGE_CURVE('',#3477,#3477,#2998,.T.);
#4214=EDGE_CURVE('',#3478,#3478,#2999,.T.);
#4215=EDGE_CURVE('',#3478,#3479,#2186,.T.);
#4216=EDGE_CURVE('',#3479,#3479,#3000,.T.);
#4217=EDGE_CURVE('',#3480,#3480,#3001,.T.);
#4218=EDGE_CURVE('',#3480,#3481,#2187,.T.);
#4219=EDGE_CURVE('',#3481,#3481,#3002,.T.);
#4220=EDGE_CURVE('',#3482,#3482,#3003,.T.);
#4221=EDGE_CURVE('',#3482,#3483,#2188,.T.);
#4222=EDGE_CURVE('',#3483,#3483,#3004,.T.);
#4223=EDGE_CURVE('',#3484,#3484,#3005,.T.);
#4224=EDGE_CURVE('',#3484,#3485,#2189,.T.);
#4225=EDGE_CURVE('',#3485,#3485,#3006,.T.);
#4226=EDGE_CURVE('',#3486,#3486,#3007,.T.);
#4227=EDGE_CURVE('',#3486,#3487,#2190,.T.);
#4228=EDGE_CURVE('',#3487,#3487,#3008,.T.);
#4229=EDGE_CURVE('',#3488,#3489,#2191,.T.);
#4230=EDGE_CURVE('',#3490,#3488,#2192,.T.);
#4231=EDGE_CURVE('',#3491,#3490,#2193,.T.);
#4232=EDGE_CURVE('',#3492,#3491,#2194,.T.);
#4233=EDGE_CURVE('',#3493,#3492,#2195,.T.);
#4234=EDGE_CURVE('',#3494,#3493,#2196,.T.);
#4235=EDGE_CURVE('',#3495,#3494,#2197,.T.);
#4236=EDGE_CURVE('',#3489,#3495,#2198,.T.);
#4237=EDGE_CURVE('',#3492,#3496,#2199,.T.);
#4238=EDGE_CURVE('',#3496,#3497,#2200,.T.);
#4239=EDGE_CURVE('',#3497,#3493,#2201,.T.);
#4240=EDGE_CURVE('',#3498,#3491,#2202,.T.);
#4241=EDGE_CURVE('',#3498,#3496,#2203,.T.);
#4242=EDGE_CURVE('',#3490,#3499,#2204,.T.);
#4243=EDGE_CURVE('',#3499,#3498,#2205,.T.);
#4244=EDGE_CURVE('',#3500,#3488,#2206,.T.);
#4245=EDGE_CURVE('',#3500,#3499,#2207,.T.);
#4246=EDGE_CURVE('',#3501,#3500,#2208,.T.);
#4247=EDGE_CURVE('',#3502,#3501,#2209,.T.);
#4248=EDGE_CURVE('',#3503,#3502,#2210,.T.);
#4249=EDGE_CURVE('',#3497,#3503,#2211,.T.);
#4250=EDGE_CURVE('',#3489,#3501,#2212,.T.);
#4251=EDGE_CURVE('',#3502,#3495,#2213,.T.);
#4252=EDGE_CURVE('',#3494,#3503,#2214,.T.);
#4253=EDGE_CURVE('',#3504,#3504,#3009,.T.);
#4254=EDGE_CURVE('',#3505,#3505,#3010,.T.);
#4255=EDGE_CURVE('',#3505,#3504,#2215,.T.);
#4256=EDGE_CURVE('',#3506,#3506,#3011,.T.);
#4257=EDGE_CURVE('',#3506,#3505,#2216,.T.);
#4258=EDGE_CURVE('',#3507,#3507,#3012,.T.);
#4259=EDGE_CURVE('',#3507,#3506,#2217,.T.);
#4260=EDGE_CURVE('',#3508,#3508,#3013,.T.);
#4261=EDGE_CURVE('',#3509,#3509,#3014,.F.);
#4262=EDGE_CURVE('',#3509,#3508,#2218,.T.);
#4263=EDGE_CURVE('',#3510,#3510,#3015,.F.);
#4264=EDGE_CURVE('',#3510,#3509,#2219,.T.);
#4265=EDGE_CURVE('',#3511,#3511,#3016,.T.);
#4266=EDGE_CURVE('',#3511,#3510,#2220,.T.);
#4267=EDGE_CURVE('',#3512,#3513,#2221,.T.);
#4268=EDGE_CURVE('',#3513,#3514,#2222,.T.);
#4269=EDGE_CURVE('',#3514,#3515,#2223,.T.);
#4270=EDGE_CURVE('',#3512,#3515,#2224,.T.);
#4271=EDGE_CURVE('',#3513,#3516,#2225,.T.);
#4272=EDGE_CURVE('',#3516,#3517,#2226,.T.);
#4273=EDGE_CURVE('',#3517,#3514,#2227,.T.);
#4274=EDGE_CURVE('',#3516,#3518,#2228,.T.);
#4275=EDGE_CURVE('',#3518,#3519,#2229,.T.);
#4276=EDGE_CURVE('',#3519,#3517,#2230,.T.);
#4277=EDGE_CURVE('',#3518,#3520,#2231,.T.);
#4278=EDGE_CURVE('',#3520,#3521,#2232,.T.);
#4279=EDGE_CURVE('',#3521,#3519,#2233,.T.);
#4280=EDGE_CURVE('',#3520,#3522,#2234,.T.);
#4281=EDGE_CURVE('',#3522,#3523,#2235,.T.);
#4282=EDGE_CURVE('',#3523,#3521,#2236,.T.);
#4283=EDGE_CURVE('',#3522,#3512,#2237,.T.);
#4284=EDGE_CURVE('',#3515,#3523,#2238,.T.);
#4285=EDGE_CURVE('',#3524,#3524,#3017,.T.);
#4286=EDGE_CURVE('',#3524,#3525,#2239,.T.);
#4287=EDGE_CURVE('',#3525,#3525,#3018,.T.);
#4288=EDGE_CURVE('',#3526,#3527,#2240,.T.);
#4289=EDGE_CURVE('',#3527,#3528,#2241,.T.);
#4290=EDGE_CURVE('',#3529,#3528,#2242,.T.);
#4291=EDGE_CURVE('',#3526,#3529,#2243,.T.);
#4292=EDGE_CURVE('',#3530,#3526,#2244,.T.);
#4293=EDGE_CURVE('',#3531,#3529,#2245,.T.);
#4294=EDGE_CURVE('',#3530,#3531,#2246,.T.);
#4295=EDGE_CURVE('',#3532,#3530,#2247,.T.);
#4296=EDGE_CURVE('',#3533,#3531,#2248,.T.);
#4297=EDGE_CURVE('',#3532,#3533,#2249,.T.);
#4298=EDGE_CURVE('',#3527,#3532,#2250,.T.);
#4299=EDGE_CURVE('',#3528,#3533,#2251,.T.);
#4300=EDGE_CURVE('',#3534,#3534,#3019,.T.);
#4301=EDGE_CURVE('',#3534,#3535,#2252,.T.);
#4302=EDGE_CURVE('',#3535,#3535,#3020,.T.);
#4303=EDGE_CURVE('',#3536,#3536,#3021,.T.);
#4304=EDGE_CURVE('',#3536,#3537,#2253,.T.);
#4305=EDGE_CURVE('',#3537,#3537,#3022,.T.);
#4306=EDGE_CURVE('',#3538,#3538,#3023,.T.);
#4307=EDGE_CURVE('',#3538,#3539,#2254,.T.);
#4308=EDGE_CURVE('',#3539,#3539,#3024,.T.);
#4309=EDGE_CURVE('',#3540,#3540,#3025,.T.);
#4310=EDGE_CURVE('',#3540,#3541,#2255,.T.);
#4311=EDGE_CURVE('',#3541,#3541,#3026,.T.);
#4312=EDGE_CURVE('',#3542,#3543,#2256,.T.);
#4313=EDGE_CURVE('',#3544,#3542,#2257,.T.);
#4314=EDGE_CURVE('',#3545,#3544,#2258,.T.);
#4315=EDGE_CURVE('',#3543,#3545,#2259,.T.);
#4316=EDGE_CURVE('',#3546,#3546,#3027,.T.);
#4317=EDGE_CURVE('',#3542,#3547,#2260,.T.);
#4318=EDGE_CURVE('',#3548,#3547,#2261,.T.);
#4319=EDGE_CURVE('',#3544,#3548,#2262,.T.);
#4320=EDGE_CURVE('',#3549,#3548,#2263,.T.);
#4321=EDGE_CURVE('',#3545,#3549,#2264,.T.);
#4322=EDGE_CURVE('',#3550,#3549,#2265,.T.);
#4323=EDGE_CURVE('',#3543,#3550,#2266,.T.);
#4324=EDGE_CURVE('',#3547,#3550,#2267,.T.);
#4325=EDGE_CURVE('',#3551,#3551,#3028,.T.);
#4326=EDGE_CURVE('',#3551,#3552,#2268,.T.);
#4327=EDGE_CURVE('',#3552,#3552,#3029,.T.);
#4328=EDGE_CURVE('',#3546,#3553,#2269,.T.);
#4329=EDGE_CURVE('',#3553,#3553,#3030,.T.);
#4330=EDGE_CURVE('',#3554,#3554,#3031,.T.);
#4331=EDGE_CURVE('',#3554,#3555,#2270,.T.);
#4332=EDGE_CURVE('',#3555,#3555,#3032,.T.);
#4333=EDGE_CURVE('',#3556,#3556,#3033,.T.);
#4334=EDGE_CURVE('',#3556,#3557,#2271,.T.);
#4335=EDGE_CURVE('',#3557,#3557,#3034,.T.);
#4336=ORIENTED_EDGE('',*,*,#3558,.F.);
#4337=ORIENTED_EDGE('',*,*,#3559,.T.);
#4338=ORIENTED_EDGE('',*,*,#3560,.F.);
#4339=ORIENTED_EDGE('',*,*,#3559,.F.);
#4340=ORIENTED_EDGE('',*,*,#3561,.F.);
#4341=ORIENTED_EDGE('',*,*,#3562,.T.);
#4342=ORIENTED_EDGE('',*,*,#3563,.F.);
#4343=ORIENTED_EDGE('',*,*,#3562,.F.);
#4344=ORIENTED_EDGE('',*,*,#3564,.F.);
#4345=ORIENTED_EDGE('',*,*,#3565,.T.);
#4346=ORIENTED_EDGE('',*,*,#3566,.F.);
#4347=ORIENTED_EDGE('',*,*,#3565,.F.);
#4348=ORIENTED_EDGE('',*,*,#3567,.F.);
#4349=ORIENTED_EDGE('',*,*,#3568,.T.);
#4350=ORIENTED_EDGE('',*,*,#3569,.F.);
#4351=ORIENTED_EDGE('',*,*,#3568,.F.);
#4352=ORIENTED_EDGE('',*,*,#3570,.F.);
#4353=ORIENTED_EDGE('',*,*,#3571,.T.);
#4354=ORIENTED_EDGE('',*,*,#3572,.F.);
#4355=ORIENTED_EDGE('',*,*,#3571,.F.);
#4356=ORIENTED_EDGE('',*,*,#3573,.F.);
#4357=ORIENTED_EDGE('',*,*,#3574,.T.);
#4358=ORIENTED_EDGE('',*,*,#3575,.F.);
#4359=ORIENTED_EDGE('',*,*,#3574,.F.);
#4360=ORIENTED_EDGE('',*,*,#3576,.F.);
#4361=ORIENTED_EDGE('',*,*,#3577,.F.);
#4362=ORIENTED_EDGE('',*,*,#3578,.F.);
#4363=ORIENTED_EDGE('',*,*,#3579,.T.);
#4364=ORIENTED_EDGE('',*,*,#3580,.F.);
#4365=ORIENTED_EDGE('',*,*,#3579,.F.);
#4366=ORIENTED_EDGE('',*,*,#3581,.F.);
#4367=ORIENTED_EDGE('',*,*,#3582,.T.);
#4368=ORIENTED_EDGE('',*,*,#3583,.F.);
#4369=ORIENTED_EDGE('',*,*,#3582,.F.);
#4370=ORIENTED_EDGE('',*,*,#3584,.F.);
#4371=ORIENTED_EDGE('',*,*,#3585,.T.);
#4372=ORIENTED_EDGE('',*,*,#3586,.F.);
#4373=ORIENTED_EDGE('',*,*,#3585,.F.);
#4374=ORIENTED_EDGE('',*,*,#3587,.F.);
#4375=ORIENTED_EDGE('',*,*,#3577,.T.);
#4376=ORIENTED_EDGE('',*,*,#3581,.T.);
#4377=ORIENTED_EDGE('',*,*,#3578,.T.);
#4378=ORIENTED_EDGE('',*,*,#3587,.T.);
#4379=ORIENTED_EDGE('',*,*,#3584,.T.);
#4380=ORIENTED_EDGE('',*,*,#3588,.T.);
#4381=ORIENTED_EDGE('',*,*,#3589,.T.);
#4382=ORIENTED_EDGE('',*,*,#3590,.F.);
#4383=ORIENTED_EDGE('',*,*,#3591,.F.);
#4384=ORIENTED_EDGE('',*,*,#3592,.T.);
#4385=ORIENTED_EDGE('',*,*,#3591,.T.);
#4386=ORIENTED_EDGE('',*,*,#3593,.F.);
#4387=ORIENTED_EDGE('',*,*,#3594,.F.);
#4388=ORIENTED_EDGE('',*,*,#3595,.T.);
#4389=ORIENTED_EDGE('',*,*,#3594,.T.);
#4390=ORIENTED_EDGE('',*,*,#3596,.F.);
#4391=ORIENTED_EDGE('',*,*,#3597,.F.);
#4392=ORIENTED_EDGE('',*,*,#3598,.T.);
#4393=ORIENTED_EDGE('',*,*,#3597,.T.);
#4394=ORIENTED_EDGE('',*,*,#3599,.F.);
#4395=ORIENTED_EDGE('',*,*,#3589,.F.);
#4396=ORIENTED_EDGE('',*,*,#3599,.T.);
#4397=ORIENTED_EDGE('',*,*,#3596,.T.);
#4398=ORIENTED_EDGE('',*,*,#3593,.T.);
#4399=ORIENTED_EDGE('',*,*,#3590,.T.);
#4400=ORIENTED_EDGE('',*,*,#3560,.T.);
#4401=ORIENTED_EDGE('',*,*,#3563,.T.);
#4402=ORIENTED_EDGE('',*,*,#3566,.T.);
#4403=ORIENTED_EDGE('',*,*,#3569,.T.);
#4404=ORIENTED_EDGE('',*,*,#3572,.T.);
#4405=ORIENTED_EDGE('',*,*,#3575,.T.);
#4406=ORIENTED_EDGE('',*,*,#3583,.T.);
#4407=ORIENTED_EDGE('',*,*,#3586,.T.);
#4408=ORIENTED_EDGE('',*,*,#3576,.T.);
#4409=ORIENTED_EDGE('',*,*,#3580,.T.);
#4410=ORIENTED_EDGE('',*,*,#3598,.F.);
#4411=ORIENTED_EDGE('',*,*,#3588,.F.);
#4412=ORIENTED_EDGE('',*,*,#3592,.F.);
#4413=ORIENTED_EDGE('',*,*,#3595,.F.);
#4414=ORIENTED_EDGE('',*,*,#3558,.T.);
#4415=ORIENTED_EDGE('',*,*,#3561,.T.);
#4416=ORIENTED_EDGE('',*,*,#3564,.T.);
#4417=ORIENTED_EDGE('',*,*,#3567,.T.);
#4418=ORIENTED_EDGE('',*,*,#3570,.T.);
#4419=ORIENTED_EDGE('',*,*,#3573,.T.);
#4420=ORIENTED_EDGE('',*,*,#3600,.T.);
#4421=ORIENTED_EDGE('',*,*,#3601,.T.);
#4422=ORIENTED_EDGE('',*,*,#3602,.F.);
#4423=ORIENTED_EDGE('',*,*,#3603,.F.);
#4424=ORIENTED_EDGE('',*,*,#3604,.T.);
#4425=ORIENTED_EDGE('',*,*,#3603,.T.);
#4426=ORIENTED_EDGE('',*,*,#3605,.F.);
#4427=ORIENTED_EDGE('',*,*,#3606,.F.);
#4428=ORIENTED_EDGE('',*,*,#3607,.T.);
#4429=ORIENTED_EDGE('',*,*,#3606,.T.);
#4430=ORIENTED_EDGE('',*,*,#3608,.F.);
#4431=ORIENTED_EDGE('',*,*,#3609,.F.);
#4432=ORIENTED_EDGE('',*,*,#3610,.T.);
#4433=ORIENTED_EDGE('',*,*,#3609,.T.);
#4434=ORIENTED_EDGE('',*,*,#3611,.F.);
#4435=ORIENTED_EDGE('',*,*,#3601,.F.);
#4436=ORIENTED_EDGE('',*,*,#3611,.T.);
#4437=ORIENTED_EDGE('',*,*,#3608,.T.);
#4438=ORIENTED_EDGE('',*,*,#3605,.T.);
#4439=ORIENTED_EDGE('',*,*,#3602,.T.);
#4440=ORIENTED_EDGE('',*,*,#3610,.F.);
#4441=ORIENTED_EDGE('',*,*,#3600,.F.);
#4442=ORIENTED_EDGE('',*,*,#3604,.F.);
#4443=ORIENTED_EDGE('',*,*,#3607,.F.);
#4444=ORIENTED_EDGE('',*,*,#3612,.T.);
#4445=ORIENTED_EDGE('',*,*,#3613,.T.);
#4446=ORIENTED_EDGE('',*,*,#3614,.F.);
#4447=ORIENTED_EDGE('',*,*,#3615,.F.);
#4448=ORIENTED_EDGE('',*,*,#3616,.T.);
#4449=ORIENTED_EDGE('',*,*,#3615,.T.);
#4450=ORIENTED_EDGE('',*,*,#3617,.F.);
#4451=ORIENTED_EDGE('',*,*,#3618,.F.);
#4452=ORIENTED_EDGE('',*,*,#3619,.T.);
#4453=ORIENTED_EDGE('',*,*,#3618,.T.);
#4454=ORIENTED_EDGE('',*,*,#3620,.F.);
#4455=ORIENTED_EDGE('',*,*,#3621,.F.);
#4456=ORIENTED_EDGE('',*,*,#3622,.T.);
#4457=ORIENTED_EDGE('',*,*,#3621,.T.);
#4458=ORIENTED_EDGE('',*,*,#3623,.F.);
#4459=ORIENTED_EDGE('',*,*,#3613,.F.);
#4460=ORIENTED_EDGE('',*,*,#3623,.T.);
#4461=ORIENTED_EDGE('',*,*,#3620,.T.);
#4462=ORIENTED_EDGE('',*,*,#3617,.T.);
#4463=ORIENTED_EDGE('',*,*,#3614,.T.);
#4464=ORIENTED_EDGE('',*,*,#3622,.F.);
#4465=ORIENTED_EDGE('',*,*,#3612,.F.);
#4466=ORIENTED_EDGE('',*,*,#3616,.F.);
#4467=ORIENTED_EDGE('',*,*,#3619,.F.);
#4468=ORIENTED_EDGE('',*,*,#3624,.F.);
#4469=ORIENTED_EDGE('',*,*,#3625,.T.);
#4470=ORIENTED_EDGE('',*,*,#3626,.F.);
#4471=ORIENTED_EDGE('',*,*,#3625,.F.);
#4472=ORIENTED_EDGE('',*,*,#3627,.F.);
#4473=ORIENTED_EDGE('',*,*,#3628,.T.);
#4474=ORIENTED_EDGE('',*,*,#3629,.F.);
#4475=ORIENTED_EDGE('',*,*,#3628,.F.);
#4476=ORIENTED_EDGE('',*,*,#3630,.F.);
#4477=ORIENTED_EDGE('',*,*,#3631,.T.);
#4478=ORIENTED_EDGE('',*,*,#3632,.F.);
#4479=ORIENTED_EDGE('',*,*,#3631,.F.);
#4480=ORIENTED_EDGE('',*,*,#3633,.F.);
#4481=ORIENTED_EDGE('',*,*,#3634,.T.);
#4482=ORIENTED_EDGE('',*,*,#3635,.F.);
#4483=ORIENTED_EDGE('',*,*,#3634,.F.);
#4484=ORIENTED_EDGE('',*,*,#3636,.F.);
#4485=ORIENTED_EDGE('',*,*,#3637,.T.);
#4486=ORIENTED_EDGE('',*,*,#3638,.F.);
#4487=ORIENTED_EDGE('',*,*,#3637,.F.);
#4488=ORIENTED_EDGE('',*,*,#3639,.F.);
#4489=ORIENTED_EDGE('',*,*,#3640,.T.);
#4490=ORIENTED_EDGE('',*,*,#3641,.F.);
#4491=ORIENTED_EDGE('',*,*,#3640,.F.);
#4492=ORIENTED_EDGE('',*,*,#3642,.F.);
#4493=ORIENTED_EDGE('',*,*,#3643,.T.);
#4494=ORIENTED_EDGE('',*,*,#3644,.F.);
#4495=ORIENTED_EDGE('',*,*,#3643,.F.);
#4496=ORIENTED_EDGE('',*,*,#3645,.F.);
#4497=ORIENTED_EDGE('',*,*,#3646,.F.);
#4498=ORIENTED_EDGE('',*,*,#3647,.T.);
#4499=ORIENTED_EDGE('',*,*,#3648,.F.);
#4500=ORIENTED_EDGE('',*,*,#3629,.T.);
#4501=ORIENTED_EDGE('',*,*,#3649,.F.);
#4502=ORIENTED_EDGE('',*,*,#3650,.F.);
#4503=ORIENTED_EDGE('',*,*,#3651,.F.);
#4504=ORIENTED_EDGE('',*,*,#3652,.F.);
#4505=ORIENTED_EDGE('',*,*,#3626,.T.);
#4506=ORIENTED_EDGE('',*,*,#3653,.F.);
#4507=ORIENTED_EDGE('',*,*,#3651,.T.);
#4508=ORIENTED_EDGE('',*,*,#3654,.F.);
#4509=ORIENTED_EDGE('',*,*,#3655,.F.);
#4510=ORIENTED_EDGE('',*,*,#3656,.F.);
#4511=ORIENTED_EDGE('',*,*,#3657,.T.);
#4512=ORIENTED_EDGE('',*,*,#3658,.F.);
#4513=ORIENTED_EDGE('',*,*,#3647,.F.);
#4514=ORIENTED_EDGE('',*,*,#3659,.T.);
#4515=ORIENTED_EDGE('',*,*,#3660,.F.);
#4516=ORIENTED_EDGE('',*,*,#3661,.F.);
#4517=ORIENTED_EDGE('',*,*,#3652,.T.);
#4518=ORIENTED_EDGE('',*,*,#3653,.T.);
#4519=ORIENTED_EDGE('',*,*,#3662,.T.);
#4520=ORIENTED_EDGE('',*,*,#3656,.T.);
#4521=ORIENTED_EDGE('',*,*,#3646,.T.);
#4522=ORIENTED_EDGE('',*,*,#3642,.T.);
#4523=ORIENTED_EDGE('',*,*,#3639,.T.);
#4524=ORIENTED_EDGE('',*,*,#3636,.T.);
#4525=ORIENTED_EDGE('',*,*,#3633,.T.);
#4526=ORIENTED_EDGE('',*,*,#3630,.T.);
#4527=ORIENTED_EDGE('',*,*,#3645,.T.);
#4528=ORIENTED_EDGE('',*,*,#3663,.T.);
#4529=ORIENTED_EDGE('',*,*,#3664,.F.);
#4530=ORIENTED_EDGE('',*,*,#3659,.F.);
#4531=ORIENTED_EDGE('',*,*,#3665,.T.);
#4532=ORIENTED_EDGE('',*,*,#3666,.F.);
#4533=ORIENTED_EDGE('',*,*,#3663,.F.);
#4534=ORIENTED_EDGE('',*,*,#3648,.T.);
#4535=ORIENTED_EDGE('',*,*,#3658,.T.);
#4536=ORIENTED_EDGE('',*,*,#3667,.T.);
#4537=ORIENTED_EDGE('',*,*,#3654,.T.);
#4538=ORIENTED_EDGE('',*,*,#3650,.T.);
#4539=ORIENTED_EDGE('',*,*,#3644,.T.);
#4540=ORIENTED_EDGE('',*,*,#3641,.T.);
#4541=ORIENTED_EDGE('',*,*,#3638,.T.);
#4542=ORIENTED_EDGE('',*,*,#3635,.T.);
#4543=ORIENTED_EDGE('',*,*,#3632,.T.);
#4544=ORIENTED_EDGE('',*,*,#3649,.T.);
#4545=ORIENTED_EDGE('',*,*,#3661,.T.);
#4546=ORIENTED_EDGE('',*,*,#3668,.F.);
#4547=ORIENTED_EDGE('',*,*,#3665,.F.);
#4548=ORIENTED_EDGE('',*,*,#3668,.T.);
#4549=ORIENTED_EDGE('',*,*,#3660,.T.);
#4550=ORIENTED_EDGE('',*,*,#3664,.T.);
#4551=ORIENTED_EDGE('',*,*,#3666,.T.);
#4552=ORIENTED_EDGE('',*,*,#3667,.F.);
#4553=ORIENTED_EDGE('',*,*,#3657,.F.);
#4554=ORIENTED_EDGE('',*,*,#3662,.F.);
#4555=ORIENTED_EDGE('',*,*,#3655,.T.);
#4556=ORIENTED_EDGE('',*,*,#3624,.T.);
#4557=ORIENTED_EDGE('',*,*,#3627,.T.);
#4558=ORIENTED_EDGE('',*,*,#3669,.F.);
#4559=ORIENTED_EDGE('',*,*,#3670,.T.);
#4560=ORIENTED_EDGE('',*,*,#3671,.F.);
#4561=ORIENTED_EDGE('',*,*,#3670,.F.);
#4562=ORIENTED_EDGE('',*,*,#3672,.F.);
#4563=ORIENTED_EDGE('',*,*,#3673,.T.);
#4564=ORIENTED_EDGE('',*,*,#3674,.F.);
#4565=ORIENTED_EDGE('',*,*,#3673,.F.);
#4566=ORIENTED_EDGE('',*,*,#3675,.F.);
#4567=ORIENTED_EDGE('',*,*,#3676,.T.);
#4568=ORIENTED_EDGE('',*,*,#3677,.F.);
#4569=ORIENTED_EDGE('',*,*,#3676,.F.);
#4570=ORIENTED_EDGE('',*,*,#3678,.F.);
#4571=ORIENTED_EDGE('',*,*,#3679,.T.);
#4572=ORIENTED_EDGE('',*,*,#3680,.F.);
#4573=ORIENTED_EDGE('',*,*,#3679,.F.);
#4574=ORIENTED_EDGE('',*,*,#3681,.F.);
#4575=ORIENTED_EDGE('',*,*,#3682,.T.);
#4576=ORIENTED_EDGE('',*,*,#3683,.F.);
#4577=ORIENTED_EDGE('',*,*,#3682,.F.);
#4578=ORIENTED_EDGE('',*,*,#3681,.T.);
#4579=ORIENTED_EDGE('',*,*,#3684,.T.);
#4580=ORIENTED_EDGE('',*,*,#3684,.F.);
#4581=ORIENTED_EDGE('',*,*,#3685,.T.);
#4582=ORIENTED_EDGE('',*,*,#3686,.T.);
#4583=ORIENTED_EDGE('',*,*,#3685,.F.);
#4584=ORIENTED_EDGE('',*,*,#3687,.F.);
#4585=ORIENTED_EDGE('',*,*,#3688,.T.);
#4586=ORIENTED_EDGE('',*,*,#3689,.T.);
#4587=ORIENTED_EDGE('',*,*,#3688,.F.);
#4588=ORIENTED_EDGE('',*,*,#3687,.T.);
#4589=ORIENTED_EDGE('',*,*,#3683,.T.);
#4590=ORIENTED_EDGE('',*,*,#3680,.T.);
#4591=ORIENTED_EDGE('',*,*,#3677,.T.);
#4592=ORIENTED_EDGE('',*,*,#3674,.T.);
#4593=ORIENTED_EDGE('',*,*,#3671,.T.);
#4594=ORIENTED_EDGE('',*,*,#3689,.F.);
#4595=ORIENTED_EDGE('',*,*,#3686,.F.);
#4596=ORIENTED_EDGE('',*,*,#3678,.T.);
#4597=ORIENTED_EDGE('',*,*,#3675,.T.);
#4598=ORIENTED_EDGE('',*,*,#3672,.T.);
#4599=ORIENTED_EDGE('',*,*,#3669,.T.);
#4600=ORIENTED_EDGE('',*,*,#3690,.F.);
#4601=ORIENTED_EDGE('',*,*,#3691,.T.);
#4602=ORIENTED_EDGE('',*,*,#3692,.F.);
#4603=ORIENTED_EDGE('',*,*,#3691,.F.);
#4604=ORIENTED_EDGE('',*,*,#3693,.F.);
#4605=ORIENTED_EDGE('',*,*,#3694,.T.);
#4606=ORIENTED_EDGE('',*,*,#3695,.F.);
#4607=ORIENTED_EDGE('',*,*,#3694,.F.);
#4608=ORIENTED_EDGE('',*,*,#3696,.F.);
#4609=ORIENTED_EDGE('',*,*,#3697,.T.);
#4610=ORIENTED_EDGE('',*,*,#3698,.F.);
#4611=ORIENTED_EDGE('',*,*,#3697,.F.);
#4612=ORIENTED_EDGE('',*,*,#3699,.F.);
#4613=ORIENTED_EDGE('',*,*,#3700,.T.);
#4614=ORIENTED_EDGE('',*,*,#3701,.F.);
#4615=ORIENTED_EDGE('',*,*,#3700,.F.);
#4616=ORIENTED_EDGE('',*,*,#3702,.F.);
#4617=ORIENTED_EDGE('',*,*,#3703,.T.);
#4618=ORIENTED_EDGE('',*,*,#3704,.T.);
#4619=ORIENTED_EDGE('',*,*,#3703,.F.);
#4620=ORIENTED_EDGE('',*,*,#3704,.F.);
#4621=ORIENTED_EDGE('',*,*,#3705,.F.);
#4622=ORIENTED_EDGE('',*,*,#3706,.F.);
#4623=ORIENTED_EDGE('',*,*,#3707,.T.);
#4624=ORIENTED_EDGE('',*,*,#3705,.T.);
#4625=ORIENTED_EDGE('',*,*,#3707,.F.);
#4626=ORIENTED_EDGE('',*,*,#3708,.F.);
#4627=ORIENTED_EDGE('',*,*,#3709,.T.);
#4628=ORIENTED_EDGE('',*,*,#3710,.T.);
#4629=ORIENTED_EDGE('',*,*,#3709,.F.);
#4630=ORIENTED_EDGE('',*,*,#3708,.T.);
#4631=ORIENTED_EDGE('',*,*,#3706,.T.);
#4632=ORIENTED_EDGE('',*,*,#3701,.T.);
#4633=ORIENTED_EDGE('',*,*,#3698,.T.);
#4634=ORIENTED_EDGE('',*,*,#3695,.T.);
#4635=ORIENTED_EDGE('',*,*,#3692,.T.);
#4636=ORIENTED_EDGE('',*,*,#3710,.F.);
#4637=ORIENTED_EDGE('',*,*,#3702,.T.);
#4638=ORIENTED_EDGE('',*,*,#3699,.T.);
#4639=ORIENTED_EDGE('',*,*,#3696,.T.);
#4640=ORIENTED_EDGE('',*,*,#3693,.T.);
#4641=ORIENTED_EDGE('',*,*,#3690,.T.);
#4642=ORIENTED_EDGE('',*,*,#3711,.F.);
#4643=ORIENTED_EDGE('',*,*,#3712,.T.);
#4644=ORIENTED_EDGE('',*,*,#3713,.F.);
#4645=ORIENTED_EDGE('',*,*,#3712,.F.);
#4646=ORIENTED_EDGE('',*,*,#3714,.F.);
#4647=ORIENTED_EDGE('',*,*,#3715,.T.);
#4648=ORIENTED_EDGE('',*,*,#3716,.F.);
#4649=ORIENTED_EDGE('',*,*,#3715,.F.);
#4650=ORIENTED_EDGE('',*,*,#3717,.F.);
#4651=ORIENTED_EDGE('',*,*,#3718,.T.);
#4652=ORIENTED_EDGE('',*,*,#3719,.F.);
#4653=ORIENTED_EDGE('',*,*,#3718,.F.);
#4654=ORIENTED_EDGE('',*,*,#3720,.F.);
#4655=ORIENTED_EDGE('',*,*,#3721,.T.);
#4656=ORIENTED_EDGE('',*,*,#3722,.F.);
#4657=ORIENTED_EDGE('',*,*,#3721,.F.);
#4658=ORIENTED_EDGE('',*,*,#3723,.F.);
#4659=ORIENTED_EDGE('',*,*,#3724,.T.);
#4660=ORIENTED_EDGE('',*,*,#3725,.F.);
#4661=ORIENTED_EDGE('',*,*,#3724,.F.);
#4662=ORIENTED_EDGE('',*,*,#3726,.F.);
#4663=ORIENTED_EDGE('',*,*,#3727,.T.);
#4664=ORIENTED_EDGE('',*,*,#3728,.F.);
#4665=ORIENTED_EDGE('',*,*,#3727,.F.);
#4666=ORIENTED_EDGE('',*,*,#3729,.F.);
#4667=ORIENTED_EDGE('',*,*,#3730,.T.);
#4668=ORIENTED_EDGE('',*,*,#3731,.F.);
#4669=ORIENTED_EDGE('',*,*,#3730,.F.);
#4670=ORIENTED_EDGE('',*,*,#3732,.F.);
#4671=ORIENTED_EDGE('',*,*,#3733,.F.);
#4672=ORIENTED_EDGE('',*,*,#3734,.T.);
#4673=ORIENTED_EDGE('',*,*,#3735,.F.);
#4674=ORIENTED_EDGE('',*,*,#3716,.T.);
#4675=ORIENTED_EDGE('',*,*,#3736,.F.);
#4676=ORIENTED_EDGE('',*,*,#3737,.F.);
#4677=ORIENTED_EDGE('',*,*,#3738,.F.);
#4678=ORIENTED_EDGE('',*,*,#3739,.F.);
#4679=ORIENTED_EDGE('',*,*,#3713,.T.);
#4680=ORIENTED_EDGE('',*,*,#3740,.F.);
#4681=ORIENTED_EDGE('',*,*,#3738,.T.);
#4682=ORIENTED_EDGE('',*,*,#3741,.F.);
#4683=ORIENTED_EDGE('',*,*,#3742,.F.);
#4684=ORIENTED_EDGE('',*,*,#3743,.F.);
#4685=ORIENTED_EDGE('',*,*,#3744,.T.);
#4686=ORIENTED_EDGE('',*,*,#3745,.F.);
#4687=ORIENTED_EDGE('',*,*,#3734,.F.);
#4688=ORIENTED_EDGE('',*,*,#3746,.T.);
#4689=ORIENTED_EDGE('',*,*,#3747,.F.);
#4690=ORIENTED_EDGE('',*,*,#3748,.F.);
#4691=ORIENTED_EDGE('',*,*,#3739,.T.);
#4692=ORIENTED_EDGE('',*,*,#3740,.T.);
#4693=ORIENTED_EDGE('',*,*,#3749,.T.);
#4694=ORIENTED_EDGE('',*,*,#3743,.T.);
#4695=ORIENTED_EDGE('',*,*,#3733,.T.);
#4696=ORIENTED_EDGE('',*,*,#3729,.T.);
#4697=ORIENTED_EDGE('',*,*,#3726,.T.);
#4698=ORIENTED_EDGE('',*,*,#3723,.T.);
#4699=ORIENTED_EDGE('',*,*,#3720,.T.);
#4700=ORIENTED_EDGE('',*,*,#3717,.T.);
#4701=ORIENTED_EDGE('',*,*,#3732,.T.);
#4702=ORIENTED_EDGE('',*,*,#3750,.T.);
#4703=ORIENTED_EDGE('',*,*,#3751,.F.);
#4704=ORIENTED_EDGE('',*,*,#3746,.F.);
#4705=ORIENTED_EDGE('',*,*,#3752,.T.);
#4706=ORIENTED_EDGE('',*,*,#3753,.F.);
#4707=ORIENTED_EDGE('',*,*,#3750,.F.);
#4708=ORIENTED_EDGE('',*,*,#3735,.T.);
#4709=ORIENTED_EDGE('',*,*,#3745,.T.);
#4710=ORIENTED_EDGE('',*,*,#3754,.T.);
#4711=ORIENTED_EDGE('',*,*,#3741,.T.);
#4712=ORIENTED_EDGE('',*,*,#3737,.T.);
#4713=ORIENTED_EDGE('',*,*,#3731,.T.);
#4714=ORIENTED_EDGE('',*,*,#3728,.T.);
#4715=ORIENTED_EDGE('',*,*,#3725,.T.);
#4716=ORIENTED_EDGE('',*,*,#3722,.T.);
#4717=ORIENTED_EDGE('',*,*,#3719,.T.);
#4718=ORIENTED_EDGE('',*,*,#3736,.T.);
#4719=ORIENTED_EDGE('',*,*,#3748,.T.);
#4720=ORIENTED_EDGE('',*,*,#3755,.F.);
#4721=ORIENTED_EDGE('',*,*,#3752,.F.);
#4722=ORIENTED_EDGE('',*,*,#3755,.T.);
#4723=ORIENTED_EDGE('',*,*,#3747,.T.);
#4724=ORIENTED_EDGE('',*,*,#3751,.T.);
#4725=ORIENTED_EDGE('',*,*,#3753,.T.);
#4726=ORIENTED_EDGE('',*,*,#3754,.F.);
#4727=ORIENTED_EDGE('',*,*,#3744,.F.);
#4728=ORIENTED_EDGE('',*,*,#3749,.F.);
#4729=ORIENTED_EDGE('',*,*,#3742,.T.);
#4730=ORIENTED_EDGE('',*,*,#3711,.T.);
#4731=ORIENTED_EDGE('',*,*,#3714,.T.);
#4732=ORIENTED_EDGE('',*,*,#3756,.F.);
#4733=ORIENTED_EDGE('',*,*,#3757,.T.);
#4734=ORIENTED_EDGE('',*,*,#3758,.F.);
#4735=ORIENTED_EDGE('',*,*,#3757,.F.);
#4736=ORIENTED_EDGE('',*,*,#3759,.F.);
#4737=ORIENTED_EDGE('',*,*,#3760,.T.);
#4738=ORIENTED_EDGE('',*,*,#3761,.F.);
#4739=ORIENTED_EDGE('',*,*,#3760,.F.);
#4740=ORIENTED_EDGE('',*,*,#3762,.F.);
#4741=ORIENTED_EDGE('',*,*,#3763,.T.);
#4742=ORIENTED_EDGE('',*,*,#3764,.F.);
#4743=ORIENTED_EDGE('',*,*,#3763,.F.);
#4744=ORIENTED_EDGE('',*,*,#3765,.F.);
#4745=ORIENTED_EDGE('',*,*,#3766,.T.);
#4746=ORIENTED_EDGE('',*,*,#3767,.F.);
#4747=ORIENTED_EDGE('',*,*,#3766,.F.);
#4748=ORIENTED_EDGE('',*,*,#3768,.F.);
#4749=ORIENTED_EDGE('',*,*,#3769,.T.);
#4750=ORIENTED_EDGE('',*,*,#3770,.F.);
#4751=ORIENTED_EDGE('',*,*,#3769,.F.);
#4752=ORIENTED_EDGE('',*,*,#3768,.T.);
#4753=ORIENTED_EDGE('',*,*,#3771,.T.);
#4754=ORIENTED_EDGE('',*,*,#3771,.F.);
#4755=ORIENTED_EDGE('',*,*,#3772,.T.);
#4756=ORIENTED_EDGE('',*,*,#3773,.T.);
#4757=ORIENTED_EDGE('',*,*,#3772,.F.);
#4758=ORIENTED_EDGE('',*,*,#3774,.F.);
#4759=ORIENTED_EDGE('',*,*,#3775,.T.);
#4760=ORIENTED_EDGE('',*,*,#3776,.T.);
#4761=ORIENTED_EDGE('',*,*,#3775,.F.);
#4762=ORIENTED_EDGE('',*,*,#3774,.T.);
#4763=ORIENTED_EDGE('',*,*,#3770,.T.);
#4764=ORIENTED_EDGE('',*,*,#3767,.T.);
#4765=ORIENTED_EDGE('',*,*,#3764,.T.);
#4766=ORIENTED_EDGE('',*,*,#3761,.T.);
#4767=ORIENTED_EDGE('',*,*,#3758,.T.);
#4768=ORIENTED_EDGE('',*,*,#3776,.F.);
#4769=ORIENTED_EDGE('',*,*,#3773,.F.);
#4770=ORIENTED_EDGE('',*,*,#3765,.T.);
#4771=ORIENTED_EDGE('',*,*,#3762,.T.);
#4772=ORIENTED_EDGE('',*,*,#3759,.T.);
#4773=ORIENTED_EDGE('',*,*,#3756,.T.);
#4774=ORIENTED_EDGE('',*,*,#3777,.F.);
#4775=ORIENTED_EDGE('',*,*,#3778,.T.);
#4776=ORIENTED_EDGE('',*,*,#3779,.F.);
#4777=ORIENTED_EDGE('',*,*,#3778,.F.);
#4778=ORIENTED_EDGE('',*,*,#3780,.F.);
#4779=ORIENTED_EDGE('',*,*,#3781,.T.);
#4780=ORIENTED_EDGE('',*,*,#3782,.F.);
#4781=ORIENTED_EDGE('',*,*,#3781,.F.);
#4782=ORIENTED_EDGE('',*,*,#3783,.F.);
#4783=ORIENTED_EDGE('',*,*,#3784,.T.);
#4784=ORIENTED_EDGE('',*,*,#3785,.F.);
#4785=ORIENTED_EDGE('',*,*,#3784,.F.);
#4786=ORIENTED_EDGE('',*,*,#3786,.F.);
#4787=ORIENTED_EDGE('',*,*,#3787,.T.);
#4788=ORIENTED_EDGE('',*,*,#3788,.F.);
#4789=ORIENTED_EDGE('',*,*,#3787,.F.);
#4790=ORIENTED_EDGE('',*,*,#3789,.F.);
#4791=ORIENTED_EDGE('',*,*,#3790,.T.);
#4792=ORIENTED_EDGE('',*,*,#3791,.T.);
#4793=ORIENTED_EDGE('',*,*,#3790,.F.);
#4794=ORIENTED_EDGE('',*,*,#3791,.F.);
#4795=ORIENTED_EDGE('',*,*,#3792,.F.);
#4796=ORIENTED_EDGE('',*,*,#3793,.F.);
#4797=ORIENTED_EDGE('',*,*,#3794,.T.);
#4798=ORIENTED_EDGE('',*,*,#3792,.T.);
#4799=ORIENTED_EDGE('',*,*,#3794,.F.);
#4800=ORIENTED_EDGE('',*,*,#3795,.F.);
#4801=ORIENTED_EDGE('',*,*,#3796,.T.);
#4802=ORIENTED_EDGE('',*,*,#3797,.T.);
#4803=ORIENTED_EDGE('',*,*,#3796,.F.);
#4804=ORIENTED_EDGE('',*,*,#3795,.T.);
#4805=ORIENTED_EDGE('',*,*,#3793,.T.);
#4806=ORIENTED_EDGE('',*,*,#3788,.T.);
#4807=ORIENTED_EDGE('',*,*,#3785,.T.);
#4808=ORIENTED_EDGE('',*,*,#3782,.T.);
#4809=ORIENTED_EDGE('',*,*,#3779,.T.);
#4810=ORIENTED_EDGE('',*,*,#3797,.F.);
#4811=ORIENTED_EDGE('',*,*,#3789,.T.);
#4812=ORIENTED_EDGE('',*,*,#3786,.T.);
#4813=ORIENTED_EDGE('',*,*,#3783,.T.);
#4814=ORIENTED_EDGE('',*,*,#3780,.T.);
#4815=ORIENTED_EDGE('',*,*,#3777,.T.);
#4816=ORIENTED_EDGE('',*,*,#3798,.F.);
#4817=ORIENTED_EDGE('',*,*,#3799,.T.);
#4818=ORIENTED_EDGE('',*,*,#3800,.F.);
#4819=ORIENTED_EDGE('',*,*,#3799,.F.);
#4820=ORIENTED_EDGE('',*,*,#3798,.T.);
#4821=ORIENTED_EDGE('',*,*,#3801,.F.);
#4822=ORIENTED_EDGE('',*,*,#3802,.T.);
#4823=ORIENTED_EDGE('',*,*,#3803,.F.);
#4824=ORIENTED_EDGE('',*,*,#3802,.F.);
#4825=ORIENTED_EDGE('',*,*,#3801,.T.);
#4826=ORIENTED_EDGE('',*,*,#3804,.F.);
#4827=ORIENTED_EDGE('',*,*,#3805,.T.);
#4828=ORIENTED_EDGE('',*,*,#3806,.F.);
#4829=ORIENTED_EDGE('',*,*,#3805,.F.);
#4830=ORIENTED_EDGE('',*,*,#3804,.T.);
#4831=ORIENTED_EDGE('',*,*,#3807,.F.);
#4832=ORIENTED_EDGE('',*,*,#3808,.T.);
#4833=ORIENTED_EDGE('',*,*,#3809,.F.);
#4834=ORIENTED_EDGE('',*,*,#3808,.F.);
#4835=ORIENTED_EDGE('',*,*,#3807,.T.);
#4836=ORIENTED_EDGE('',*,*,#3810,.F.);
#4837=ORIENTED_EDGE('',*,*,#3811,.T.);
#4838=ORIENTED_EDGE('',*,*,#3812,.F.);
#4839=ORIENTED_EDGE('',*,*,#3811,.F.);
#4840=ORIENTED_EDGE('',*,*,#3810,.T.);
#4841=ORIENTED_EDGE('',*,*,#3813,.F.);
#4842=ORIENTED_EDGE('',*,*,#3814,.F.);
#4843=ORIENTED_EDGE('',*,*,#3815,.T.);
#4844=ORIENTED_EDGE('',*,*,#3813,.T.);
#4845=ORIENTED_EDGE('',*,*,#3815,.F.);
#4846=ORIENTED_EDGE('',*,*,#3816,.F.);
#4847=ORIENTED_EDGE('',*,*,#3817,.T.);
#4848=ORIENTED_EDGE('',*,*,#3818,.F.);
#4849=ORIENTED_EDGE('',*,*,#3817,.F.);
#4850=ORIENTED_EDGE('',*,*,#3816,.T.);
#4851=ORIENTED_EDGE('',*,*,#3819,.F.);
#4852=ORIENTED_EDGE('',*,*,#3820,.F.);
#4853=ORIENTED_EDGE('',*,*,#3821,.T.);
#4854=ORIENTED_EDGE('',*,*,#3819,.T.);
#4855=ORIENTED_EDGE('',*,*,#3821,.F.);
#4856=ORIENTED_EDGE('',*,*,#3822,.F.);
#4857=ORIENTED_EDGE('',*,*,#3823,.T.);
#4858=ORIENTED_EDGE('',*,*,#3824,.F.);
#4859=ORIENTED_EDGE('',*,*,#3823,.F.);
#4860=ORIENTED_EDGE('',*,*,#3822,.T.);
#4861=ORIENTED_EDGE('',*,*,#3825,.F.);
#4862=ORIENTED_EDGE('',*,*,#3826,.F.);
#4863=ORIENTED_EDGE('',*,*,#3827,.T.);
#4864=ORIENTED_EDGE('',*,*,#3825,.T.);
#4865=ORIENTED_EDGE('',*,*,#3827,.F.);
#4866=ORIENTED_EDGE('',*,*,#3828,.F.);
#4867=ORIENTED_EDGE('',*,*,#3829,.T.);
#4868=ORIENTED_EDGE('',*,*,#3830,.F.);
#4869=ORIENTED_EDGE('',*,*,#3831,.F.);
#4870=ORIENTED_EDGE('',*,*,#3832,.F.);
#4871=ORIENTED_EDGE('',*,*,#3833,.F.);
#4872=ORIENTED_EDGE('',*,*,#3834,.F.);
#4873=ORIENTED_EDGE('',*,*,#3835,.F.);
#4874=ORIENTED_EDGE('',*,*,#3836,.F.);
#4875=ORIENTED_EDGE('',*,*,#3837,.T.);
#4876=ORIENTED_EDGE('',*,*,#3838,.F.);
#4877=ORIENTED_EDGE('',*,*,#3839,.F.);
#4878=ORIENTED_EDGE('',*,*,#3814,.T.);
#4879=ORIENTED_EDGE('',*,*,#3840,.T.);
#4880=ORIENTED_EDGE('',*,*,#3841,.T.);
#4881=ORIENTED_EDGE('',*,*,#3830,.T.);
#4882=ORIENTED_EDGE('',*,*,#3842,.T.);
#4883=ORIENTED_EDGE('',*,*,#3843,.T.);
#4884=ORIENTED_EDGE('',*,*,#3844,.T.);
#4885=ORIENTED_EDGE('',*,*,#3836,.T.);
#4886=ORIENTED_EDGE('',*,*,#3845,.T.);
#4887=ORIENTED_EDGE('',*,*,#3833,.T.);
#4888=ORIENTED_EDGE('',*,*,#3846,.F.);
#4889=ORIENTED_EDGE('',*,*,#3847,.F.);
#4890=ORIENTED_EDGE('',*,*,#3848,.F.);
#4891=ORIENTED_EDGE('',*,*,#3832,.T.);
#4892=ORIENTED_EDGE('',*,*,#3849,.T.);
#4893=ORIENTED_EDGE('',*,*,#3850,.T.);
#4894=ORIENTED_EDGE('',*,*,#3846,.T.);
#4895=ORIENTED_EDGE('',*,*,#3851,.F.);
#4896=ORIENTED_EDGE('',*,*,#3847,.T.);
#4897=ORIENTED_EDGE('',*,*,#3850,.F.);
#4898=ORIENTED_EDGE('',*,*,#3852,.F.);
#4899=ORIENTED_EDGE('',*,*,#3820,.T.);
#4900=ORIENTED_EDGE('',*,*,#3853,.F.);
#4901=ORIENTED_EDGE('',*,*,#3852,.T.);
#4902=ORIENTED_EDGE('',*,*,#3849,.F.);
#4903=ORIENTED_EDGE('',*,*,#3831,.T.);
#4904=ORIENTED_EDGE('',*,*,#3841,.F.);
#4905=ORIENTED_EDGE('',*,*,#3854,.F.);
#4906=ORIENTED_EDGE('',*,*,#3845,.F.);
#4907=ORIENTED_EDGE('',*,*,#3835,.T.);
#4908=ORIENTED_EDGE('',*,*,#3834,.T.);
#4909=ORIENTED_EDGE('',*,*,#3848,.T.);
#4910=ORIENTED_EDGE('',*,*,#3851,.T.);
#4911=ORIENTED_EDGE('',*,*,#3853,.T.);
#4912=ORIENTED_EDGE('',*,*,#3839,.T.);
#4913=ORIENTED_EDGE('',*,*,#3855,.F.);
#4914=ORIENTED_EDGE('',*,*,#3856,.T.);
#4915=ORIENTED_EDGE('',*,*,#3857,.T.);
#4916=ORIENTED_EDGE('',*,*,#3838,.T.);
#4917=ORIENTED_EDGE('',*,*,#3858,.F.);
#4918=ORIENTED_EDGE('',*,*,#3859,.T.);
#4919=ORIENTED_EDGE('',*,*,#3855,.T.);
#4920=ORIENTED_EDGE('',*,*,#3828,.T.);
#4921=ORIENTED_EDGE('',*,*,#3857,.F.);
#4922=ORIENTED_EDGE('',*,*,#3860,.T.);
#4923=ORIENTED_EDGE('',*,*,#3861,.T.);
#4924=ORIENTED_EDGE('',*,*,#3861,.F.);
#4925=ORIENTED_EDGE('',*,*,#3862,.T.);
#4926=ORIENTED_EDGE('',*,*,#3858,.T.);
#4927=ORIENTED_EDGE('',*,*,#3837,.F.);
#4928=ORIENTED_EDGE('',*,*,#3844,.F.);
#4929=ORIENTED_EDGE('',*,*,#3863,.T.);
#4930=ORIENTED_EDGE('',*,*,#3842,.F.);
#4931=ORIENTED_EDGE('',*,*,#3829,.F.);
#4932=ORIENTED_EDGE('',*,*,#3863,.F.);
#4933=ORIENTED_EDGE('',*,*,#3843,.F.);
#4934=ORIENTED_EDGE('',*,*,#3854,.T.);
#4935=ORIENTED_EDGE('',*,*,#3840,.F.);
#4936=ORIENTED_EDGE('',*,*,#3824,.T.);
#4937=ORIENTED_EDGE('',*,*,#3818,.T.);
#4938=ORIENTED_EDGE('',*,*,#3812,.T.);
#4939=ORIENTED_EDGE('',*,*,#3809,.T.);
#4940=ORIENTED_EDGE('',*,*,#3806,.T.);
#4941=ORIENTED_EDGE('',*,*,#3803,.T.);
#4942=ORIENTED_EDGE('',*,*,#3800,.T.);
#4943=ORIENTED_EDGE('',*,*,#3862,.F.);
#4944=ORIENTED_EDGE('',*,*,#3860,.F.);
#4945=ORIENTED_EDGE('',*,*,#3856,.F.);
#4946=ORIENTED_EDGE('',*,*,#3859,.F.);
#4947=ORIENTED_EDGE('',*,*,#3826,.T.);
#4948=ORIENTED_EDGE('',*,*,#3864,.F.);
#4949=ORIENTED_EDGE('',*,*,#3865,.T.);
#4950=ORIENTED_EDGE('',*,*,#3866,.T.);
#4951=ORIENTED_EDGE('',*,*,#3865,.F.);
#4952=ORIENTED_EDGE('',*,*,#3867,.F.);
#4953=ORIENTED_EDGE('',*,*,#3868,.T.);
#4954=ORIENTED_EDGE('',*,*,#3869,.T.);
#4955=ORIENTED_EDGE('',*,*,#3868,.F.);
#4956=ORIENTED_EDGE('',*,*,#3867,.T.);
#4957=ORIENTED_EDGE('',*,*,#3864,.T.);
#4958=ORIENTED_EDGE('',*,*,#3869,.F.);
#4959=ORIENTED_EDGE('',*,*,#3866,.F.);
#4960=ORIENTED_EDGE('',*,*,#3870,.F.);
#4961=ORIENTED_EDGE('',*,*,#3871,.T.);
#4962=ORIENTED_EDGE('',*,*,#3872,.F.);
#4963=ORIENTED_EDGE('',*,*,#3871,.F.);
#4964=ORIENTED_EDGE('',*,*,#3873,.F.);
#4965=ORIENTED_EDGE('',*,*,#3874,.T.);
#4966=ORIENTED_EDGE('',*,*,#3875,.F.);
#4967=ORIENTED_EDGE('',*,*,#3874,.F.);
#4968=ORIENTED_EDGE('',*,*,#3876,.F.);
#4969=ORIENTED_EDGE('',*,*,#3877,.T.);
#4970=ORIENTED_EDGE('',*,*,#3878,.F.);
#4971=ORIENTED_EDGE('',*,*,#3877,.F.);
#4972=ORIENTED_EDGE('',*,*,#3879,.F.);
#4973=ORIENTED_EDGE('',*,*,#3880,.T.);
#4974=ORIENTED_EDGE('',*,*,#3881,.F.);
#4975=ORIENTED_EDGE('',*,*,#3880,.F.);
#4976=ORIENTED_EDGE('',*,*,#3882,.F.);
#4977=ORIENTED_EDGE('',*,*,#3883,.T.);
#4978=ORIENTED_EDGE('',*,*,#3884,.T.);
#4979=ORIENTED_EDGE('',*,*,#3883,.F.);
#4980=ORIENTED_EDGE('',*,*,#3884,.F.);
#4981=ORIENTED_EDGE('',*,*,#3885,.F.);
#4982=ORIENTED_EDGE('',*,*,#3886,.F.);
#4983=ORIENTED_EDGE('',*,*,#3887,.T.);
#4984=ORIENTED_EDGE('',*,*,#3885,.T.);
#4985=ORIENTED_EDGE('',*,*,#3887,.F.);
#4986=ORIENTED_EDGE('',*,*,#3888,.F.);
#4987=ORIENTED_EDGE('',*,*,#3889,.T.);
#4988=ORIENTED_EDGE('',*,*,#3890,.T.);
#4989=ORIENTED_EDGE('',*,*,#3889,.F.);
#4990=ORIENTED_EDGE('',*,*,#3888,.T.);
#4991=ORIENTED_EDGE('',*,*,#3886,.T.);
#4992=ORIENTED_EDGE('',*,*,#3881,.T.);
#4993=ORIENTED_EDGE('',*,*,#3878,.T.);
#4994=ORIENTED_EDGE('',*,*,#3875,.T.);
#4995=ORIENTED_EDGE('',*,*,#3872,.T.);
#4996=ORIENTED_EDGE('',*,*,#3890,.F.);
#4997=ORIENTED_EDGE('',*,*,#3882,.T.);
#4998=ORIENTED_EDGE('',*,*,#3879,.T.);
#4999=ORIENTED_EDGE('',*,*,#3876,.T.);
#5000=ORIENTED_EDGE('',*,*,#3873,.T.);
#5001=ORIENTED_EDGE('',*,*,#3870,.T.);
#5002=ORIENTED_EDGE('',*,*,#3891,.T.);
#5003=ORIENTED_EDGE('',*,*,#3892,.T.);
#5004=ORIENTED_EDGE('',*,*,#3893,.F.);
#5005=ORIENTED_EDGE('',*,*,#3892,.F.);
#5006=ORIENTED_EDGE('',*,*,#3893,.T.);
#5007=ORIENTED_EDGE('',*,*,#3891,.F.);
#5008=ORIENTED_EDGE('',*,*,#3894,.F.);
#5009=ORIENTED_EDGE('',*,*,#3895,.F.);
#5010=ORIENTED_EDGE('',*,*,#3896,.T.);
#5011=ORIENTED_EDGE('',*,*,#3897,.F.);
#5012=ORIENTED_EDGE('',*,*,#3898,.F.);
#5013=ORIENTED_EDGE('',*,*,#3896,.F.);
#5014=ORIENTED_EDGE('',*,*,#3897,.T.);
#5015=ORIENTED_EDGE('',*,*,#3898,.T.);
#5016=ORIENTED_EDGE('',*,*,#3899,.T.);
#5017=ORIENTED_EDGE('',*,*,#3900,.T.);
#5018=ORIENTED_EDGE('',*,*,#3899,.F.);
#5019=ORIENTED_EDGE('',*,*,#3901,.T.);
#5020=ORIENTED_EDGE('',*,*,#3902,.T.);
#5021=ORIENTED_EDGE('',*,*,#3903,.F.);
#5022=ORIENTED_EDGE('',*,*,#3902,.F.);
#5023=ORIENTED_EDGE('',*,*,#3903,.T.);
#5024=ORIENTED_EDGE('',*,*,#3904,.T.);
#5025=ORIENTED_EDGE('',*,*,#3905,.F.);
#5026=ORIENTED_EDGE('',*,*,#3904,.F.);
#5027=ORIENTED_EDGE('',*,*,#3900,.F.);
#5028=ORIENTED_EDGE('',*,*,#3905,.T.);
#5029=ORIENTED_EDGE('',*,*,#3906,.F.);
#5030=ORIENTED_EDGE('',*,*,#3907,.T.);
#5031=ORIENTED_EDGE('',*,*,#3894,.T.);
#5032=ORIENTED_EDGE('',*,*,#3895,.T.);
#5033=ORIENTED_EDGE('',*,*,#3907,.F.);
#5034=ORIENTED_EDGE('',*,*,#3906,.T.);
#5035=ORIENTED_EDGE('',*,*,#3908,.F.);
#5036=ORIENTED_EDGE('',*,*,#3908,.T.);
#5037=ORIENTED_EDGE('',*,*,#3909,.T.);
#5038=ORIENTED_EDGE('',*,*,#3901,.F.);
#5039=ORIENTED_EDGE('',*,*,#3909,.F.);
#5040=ORIENTED_EDGE('',*,*,#3910,.F.);
#5041=ORIENTED_EDGE('',*,*,#3911,.F.);
#5042=ORIENTED_EDGE('',*,*,#3912,.T.);
#5043=ORIENTED_EDGE('',*,*,#3913,.F.);
#5044=ORIENTED_EDGE('',*,*,#3914,.F.);
#5045=ORIENTED_EDGE('',*,*,#3912,.F.);
#5046=ORIENTED_EDGE('',*,*,#3915,.T.);
#5047=ORIENTED_EDGE('',*,*,#3916,.T.);
#5048=ORIENTED_EDGE('',*,*,#3913,.T.);
#5049=ORIENTED_EDGE('',*,*,#3914,.T.);
#5050=ORIENTED_EDGE('',*,*,#3916,.F.);
#5051=ORIENTED_EDGE('',*,*,#3917,.F.);
#5052=ORIENTED_EDGE('',*,*,#3918,.T.);
#5053=ORIENTED_EDGE('',*,*,#3919,.F.);
#5054=ORIENTED_EDGE('',*,*,#3920,.T.);
#5055=ORIENTED_EDGE('',*,*,#3917,.T.);
#5056=ORIENTED_EDGE('',*,*,#3920,.F.);
#5057=ORIENTED_EDGE('',*,*,#3921,.F.);
#5058=ORIENTED_EDGE('',*,*,#3922,.T.);
#5059=ORIENTED_EDGE('',*,*,#3919,.T.);
#5060=ORIENTED_EDGE('',*,*,#3922,.F.);
#5061=ORIENTED_EDGE('',*,*,#3923,.F.);
#5062=ORIENTED_EDGE('',*,*,#3924,.T.);
#5063=ORIENTED_EDGE('',*,*,#3921,.T.);
#5064=ORIENTED_EDGE('',*,*,#3924,.F.);
#5065=ORIENTED_EDGE('',*,*,#3923,.T.);
#5066=ORIENTED_EDGE('',*,*,#3915,.F.);
#5067=ORIENTED_EDGE('',*,*,#3910,.T.);
#5068=ORIENTED_EDGE('',*,*,#3911,.T.);
#5069=ORIENTED_EDGE('',*,*,#3925,.T.);
#5070=ORIENTED_EDGE('',*,*,#3918,.F.);
#5071=ORIENTED_EDGE('',*,*,#3925,.F.);
#5072=ORIENTED_EDGE('',*,*,#3926,.T.);
#5073=ORIENTED_EDGE('',*,*,#3926,.F.);
#5074=ORIENTED_EDGE('',*,*,#3927,.T.);
#5075=ORIENTED_EDGE('',*,*,#3927,.F.);
#5076=ORIENTED_EDGE('',*,*,#3928,.T.);
#5077=ORIENTED_EDGE('',*,*,#3928,.F.);
#5078=ORIENTED_EDGE('',*,*,#3929,.T.);
#5079=ORIENTED_EDGE('',*,*,#3929,.F.);
#5080=ORIENTED_EDGE('',*,*,#3930,.T.);
#5081=ORIENTED_EDGE('',*,*,#3930,.F.);
#5082=ORIENTED_EDGE('',*,*,#3931,.T.);
#5083=ORIENTED_EDGE('',*,*,#3931,.F.);
#5084=ORIENTED_EDGE('',*,*,#3932,.T.);
#5085=ORIENTED_EDGE('',*,*,#3932,.F.);
#5086=ORIENTED_EDGE('',*,*,#3933,.F.);
#5087=ORIENTED_EDGE('',*,*,#3934,.F.);
#5088=ORIENTED_EDGE('',*,*,#3935,.F.);
#5089=ORIENTED_EDGE('',*,*,#3936,.F.);
#5090=ORIENTED_EDGE('',*,*,#3935,.T.);
#5091=ORIENTED_EDGE('',*,*,#3937,.F.);
#5092=ORIENTED_EDGE('',*,*,#3938,.T.);
#5093=ORIENTED_EDGE('',*,*,#3939,.F.);
#5094=ORIENTED_EDGE('',*,*,#3940,.T.);
#5095=ORIENTED_EDGE('',*,*,#3941,.F.);
#5096=ORIENTED_EDGE('',*,*,#3942,.T.);
#5097=ORIENTED_EDGE('',*,*,#3943,.F.);
#5098=ORIENTED_EDGE('',*,*,#3942,.F.);
#5099=ORIENTED_EDGE('',*,*,#3944,.F.);
#5100=ORIENTED_EDGE('',*,*,#3945,.T.);
#5101=ORIENTED_EDGE('',*,*,#3946,.F.);
#5102=ORIENTED_EDGE('',*,*,#3947,.T.);
#5103=ORIENTED_EDGE('',*,*,#3948,.F.);
#5104=ORIENTED_EDGE('',*,*,#3949,.T.);
#5105=ORIENTED_EDGE('',*,*,#3950,.F.);
#5106=ORIENTED_EDGE('',*,*,#3951,.T.);
#5107=ORIENTED_EDGE('',*,*,#3952,.F.);
#5108=ORIENTED_EDGE('',*,*,#3934,.T.);
#5109=ORIENTED_EDGE('',*,*,#3953,.T.);
#5110=ORIENTED_EDGE('',*,*,#3954,.T.);
#5111=ORIENTED_EDGE('',*,*,#3937,.T.);
#5112=ORIENTED_EDGE('',*,*,#3955,.F.);
#5113=ORIENTED_EDGE('',*,*,#3956,.F.);
#5114=ORIENTED_EDGE('',*,*,#3938,.F.);
#5115=ORIENTED_EDGE('',*,*,#3954,.F.);
#5116=ORIENTED_EDGE('',*,*,#3956,.T.);
#5117=ORIENTED_EDGE('',*,*,#3957,.T.);
#5118=ORIENTED_EDGE('',*,*,#3958,.T.);
#5119=ORIENTED_EDGE('',*,*,#3939,.T.);
#5120=ORIENTED_EDGE('',*,*,#3959,.F.);
#5121=ORIENTED_EDGE('',*,*,#3960,.F.);
#5122=ORIENTED_EDGE('',*,*,#3940,.F.);
#5123=ORIENTED_EDGE('',*,*,#3958,.F.);
#5124=ORIENTED_EDGE('',*,*,#3960,.T.);
#5125=ORIENTED_EDGE('',*,*,#3961,.T.);
#5126=ORIENTED_EDGE('',*,*,#3962,.T.);
#5127=ORIENTED_EDGE('',*,*,#3963,.T.);
#5128=ORIENTED_EDGE('',*,*,#3944,.T.);
#5129=ORIENTED_EDGE('',*,*,#3941,.T.);
#5130=ORIENTED_EDGE('',*,*,#3964,.F.);
#5131=ORIENTED_EDGE('',*,*,#3965,.F.);
#5132=ORIENTED_EDGE('',*,*,#3945,.F.);
#5133=ORIENTED_EDGE('',*,*,#3963,.F.);
#5134=ORIENTED_EDGE('',*,*,#3965,.T.);
#5135=ORIENTED_EDGE('',*,*,#3966,.T.);
#5136=ORIENTED_EDGE('',*,*,#3967,.T.);
#5137=ORIENTED_EDGE('',*,*,#3946,.T.);
#5138=ORIENTED_EDGE('',*,*,#3968,.F.);
#5139=ORIENTED_EDGE('',*,*,#3969,.F.);
#5140=ORIENTED_EDGE('',*,*,#3947,.F.);
#5141=ORIENTED_EDGE('',*,*,#3967,.F.);
#5142=ORIENTED_EDGE('',*,*,#3969,.T.);
#5143=ORIENTED_EDGE('',*,*,#3970,.T.);
#5144=ORIENTED_EDGE('',*,*,#3971,.T.);
#5145=ORIENTED_EDGE('',*,*,#3948,.T.);
#5146=ORIENTED_EDGE('',*,*,#3949,.F.);
#5147=ORIENTED_EDGE('',*,*,#3971,.F.);
#5148=ORIENTED_EDGE('',*,*,#3972,.F.);
#5149=ORIENTED_EDGE('',*,*,#3973,.F.);
#5150=ORIENTED_EDGE('',*,*,#3974,.F.);
#5151=ORIENTED_EDGE('',*,*,#3975,.T.);
#5152=ORIENTED_EDGE('',*,*,#3961,.F.);
#5153=ORIENTED_EDGE('',*,*,#3959,.T.);
#5154=ORIENTED_EDGE('',*,*,#3957,.F.);
#5155=ORIENTED_EDGE('',*,*,#3955,.T.);
#5156=ORIENTED_EDGE('',*,*,#3953,.F.);
#5157=ORIENTED_EDGE('',*,*,#3933,.T.);
#5158=ORIENTED_EDGE('',*,*,#3976,.F.);
#5159=ORIENTED_EDGE('',*,*,#3977,.T.);
#5160=ORIENTED_EDGE('',*,*,#3978,.F.);
#5161=ORIENTED_EDGE('',*,*,#3972,.T.);
#5162=ORIENTED_EDGE('',*,*,#3970,.F.);
#5163=ORIENTED_EDGE('',*,*,#3968,.T.);
#5164=ORIENTED_EDGE('',*,*,#3966,.F.);
#5165=ORIENTED_EDGE('',*,*,#3964,.T.);
#5166=ORIENTED_EDGE('',*,*,#3962,.F.);
#5167=ORIENTED_EDGE('',*,*,#3975,.F.);
#5168=ORIENTED_EDGE('',*,*,#3936,.T.);
#5169=ORIENTED_EDGE('',*,*,#3952,.T.);
#5170=ORIENTED_EDGE('',*,*,#3979,.T.);
#5171=ORIENTED_EDGE('',*,*,#3976,.T.);
#5172=ORIENTED_EDGE('',*,*,#3951,.F.);
#5173=ORIENTED_EDGE('',*,*,#3980,.F.);
#5174=ORIENTED_EDGE('',*,*,#3977,.F.);
#5175=ORIENTED_EDGE('',*,*,#3979,.F.);
#5176=ORIENTED_EDGE('',*,*,#3943,.T.);
#5177=ORIENTED_EDGE('',*,*,#3974,.T.);
#5178=ORIENTED_EDGE('',*,*,#3973,.T.);
#5179=ORIENTED_EDGE('',*,*,#3978,.T.);
#5180=ORIENTED_EDGE('',*,*,#3980,.T.);
#5181=ORIENTED_EDGE('',*,*,#3950,.T.);
#5182=ORIENTED_EDGE('',*,*,#3981,.F.);
#5183=ORIENTED_EDGE('',*,*,#3982,.T.);
#5184=ORIENTED_EDGE('',*,*,#3983,.F.);
#5185=ORIENTED_EDGE('',*,*,#3984,.T.);
#5186=ORIENTED_EDGE('',*,*,#3981,.T.);
#5187=ORIENTED_EDGE('',*,*,#3984,.F.);
#5188=ORIENTED_EDGE('',*,*,#3983,.T.);
#5189=ORIENTED_EDGE('',*,*,#3985,.F.);
#5190=ORIENTED_EDGE('',*,*,#3985,.T.);
#5191=ORIENTED_EDGE('',*,*,#3986,.T.);
#5192=ORIENTED_EDGE('',*,*,#3982,.F.);
#5193=ORIENTED_EDGE('',*,*,#3986,.F.);
#5194=ORIENTED_EDGE('',*,*,#3987,.F.);
#5195=ORIENTED_EDGE('',*,*,#3988,.T.);
#5196=ORIENTED_EDGE('',*,*,#3989,.F.);
#5197=ORIENTED_EDGE('',*,*,#3990,.T.);
#5198=ORIENTED_EDGE('',*,*,#3987,.T.);
#5199=ORIENTED_EDGE('',*,*,#3990,.F.);
#5200=ORIENTED_EDGE('',*,*,#3989,.T.);
#5201=ORIENTED_EDGE('',*,*,#3991,.F.);
#5202=ORIENTED_EDGE('',*,*,#3991,.T.);
#5203=ORIENTED_EDGE('',*,*,#3992,.T.);
#5204=ORIENTED_EDGE('',*,*,#3988,.F.);
#5205=ORIENTED_EDGE('',*,*,#3992,.F.);
#5206=ORIENTED_EDGE('',*,*,#3993,.F.);
#5207=ORIENTED_EDGE('',*,*,#3994,.F.);
#5208=ORIENTED_EDGE('',*,*,#3995,.T.);
#5209=ORIENTED_EDGE('',*,*,#3993,.T.);
#5210=ORIENTED_EDGE('',*,*,#3995,.F.);
#5211=ORIENTED_EDGE('',*,*,#3996,.F.);
#5212=ORIENTED_EDGE('',*,*,#3997,.T.);
#5213=ORIENTED_EDGE('',*,*,#3994,.T.);
#5214=ORIENTED_EDGE('',*,*,#3997,.F.);
#5215=ORIENTED_EDGE('',*,*,#3998,.F.);
#5216=ORIENTED_EDGE('',*,*,#3999,.T.);
#5217=ORIENTED_EDGE('',*,*,#3996,.T.);
#5218=ORIENTED_EDGE('',*,*,#3999,.F.);
#5219=ORIENTED_EDGE('',*,*,#3998,.T.);
#5220=ORIENTED_EDGE('',*,*,#4000,.F.);
#5221=ORIENTED_EDGE('',*,*,#4001,.F.);
#5222=ORIENTED_EDGE('',*,*,#4002,.T.);
#5223=ORIENTED_EDGE('',*,*,#4000,.T.);
#5224=ORIENTED_EDGE('',*,*,#4002,.F.);
#5225=ORIENTED_EDGE('',*,*,#4003,.F.);
#5226=ORIENTED_EDGE('',*,*,#4004,.T.);
#5227=ORIENTED_EDGE('',*,*,#4001,.T.);
#5228=ORIENTED_EDGE('',*,*,#4004,.F.);
#5229=ORIENTED_EDGE('',*,*,#4005,.F.);
#5230=ORIENTED_EDGE('',*,*,#4006,.T.);
#5231=ORIENTED_EDGE('',*,*,#4003,.T.);
#5232=ORIENTED_EDGE('',*,*,#4006,.F.);
#5233=ORIENTED_EDGE('',*,*,#4005,.T.);
#5234=ORIENTED_EDGE('',*,*,#4007,.T.);
#5235=ORIENTED_EDGE('',*,*,#4008,.T.);
#5236=ORIENTED_EDGE('',*,*,#4009,.T.);
#5237=ORIENTED_EDGE('',*,*,#4010,.F.);
#5238=ORIENTED_EDGE('',*,*,#4011,.T.);
#5239=ORIENTED_EDGE('',*,*,#4012,.T.);
#5240=ORIENTED_EDGE('',*,*,#4013,.T.);
#5241=ORIENTED_EDGE('',*,*,#4008,.F.);
#5242=ORIENTED_EDGE('',*,*,#4014,.T.);
#5243=ORIENTED_EDGE('',*,*,#4015,.T.);
#5244=ORIENTED_EDGE('',*,*,#4016,.T.);
#5245=ORIENTED_EDGE('',*,*,#4012,.F.);
#5246=ORIENTED_EDGE('',*,*,#4017,.T.);
#5247=ORIENTED_EDGE('',*,*,#4018,.T.);
#5248=ORIENTED_EDGE('',*,*,#4019,.T.);
#5249=ORIENTED_EDGE('',*,*,#4015,.F.);
#5250=ORIENTED_EDGE('',*,*,#4020,.T.);
#5251=ORIENTED_EDGE('',*,*,#4021,.T.);
#5252=ORIENTED_EDGE('',*,*,#4022,.T.);
#5253=ORIENTED_EDGE('',*,*,#4018,.F.);
#5254=ORIENTED_EDGE('',*,*,#4023,.T.);
#5255=ORIENTED_EDGE('',*,*,#4010,.T.);
#5256=ORIENTED_EDGE('',*,*,#4024,.T.);
#5257=ORIENTED_EDGE('',*,*,#4021,.F.);
#5258=ORIENTED_EDGE('',*,*,#4023,.F.);
#5259=ORIENTED_EDGE('',*,*,#4020,.F.);
#5260=ORIENTED_EDGE('',*,*,#4017,.F.);
#5261=ORIENTED_EDGE('',*,*,#4014,.F.);
#5262=ORIENTED_EDGE('',*,*,#4011,.F.);
#5263=ORIENTED_EDGE('',*,*,#4007,.F.);
#5264=ORIENTED_EDGE('',*,*,#4024,.F.);
#5265=ORIENTED_EDGE('',*,*,#4009,.F.);
#5266=ORIENTED_EDGE('',*,*,#4013,.F.);
#5267=ORIENTED_EDGE('',*,*,#4016,.F.);
#5268=ORIENTED_EDGE('',*,*,#4019,.F.);
#5269=ORIENTED_EDGE('',*,*,#4022,.F.);
#5270=ORIENTED_EDGE('',*,*,#4025,.F.);
#5271=ORIENTED_EDGE('',*,*,#4026,.F.);
#5272=ORIENTED_EDGE('',*,*,#4027,.F.);
#5273=ORIENTED_EDGE('',*,*,#4028,.F.);
#5274=ORIENTED_EDGE('',*,*,#4029,.F.);
#5275=ORIENTED_EDGE('',*,*,#4028,.T.);
#5276=ORIENTED_EDGE('',*,*,#4030,.F.);
#5277=ORIENTED_EDGE('',*,*,#4031,.T.);
#5278=ORIENTED_EDGE('',*,*,#4032,.F.);
#5279=ORIENTED_EDGE('',*,*,#4031,.F.);
#5280=ORIENTED_EDGE('',*,*,#4033,.F.);
#5281=ORIENTED_EDGE('',*,*,#4034,.F.);
#5282=ORIENTED_EDGE('',*,*,#4035,.F.);
#5283=ORIENTED_EDGE('',*,*,#4034,.T.);
#5284=ORIENTED_EDGE('',*,*,#4036,.T.);
#5285=ORIENTED_EDGE('',*,*,#4026,.T.);
#5286=ORIENTED_EDGE('',*,*,#4036,.F.);
#5287=ORIENTED_EDGE('',*,*,#4033,.T.);
#5288=ORIENTED_EDGE('',*,*,#4030,.T.);
#5289=ORIENTED_EDGE('',*,*,#4027,.T.);
#5290=ORIENTED_EDGE('',*,*,#4037,.F.);
#5291=ORIENTED_EDGE('',*,*,#4038,.T.);
#5292=ORIENTED_EDGE('',*,*,#4039,.F.);
#5293=ORIENTED_EDGE('',*,*,#4040,.T.);
#5294=ORIENTED_EDGE('',*,*,#4037,.T.);
#5295=ORIENTED_EDGE('',*,*,#4040,.F.);
#5296=ORIENTED_EDGE('',*,*,#4039,.T.);
#5297=ORIENTED_EDGE('',*,*,#4041,.F.);
#5298=ORIENTED_EDGE('',*,*,#4042,.F.);
#5299=ORIENTED_EDGE('',*,*,#4043,.T.);
#5300=ORIENTED_EDGE('',*,*,#4041,.T.);
#5301=ORIENTED_EDGE('',*,*,#4043,.F.);
#5302=ORIENTED_EDGE('',*,*,#4044,.F.);
#5303=ORIENTED_EDGE('',*,*,#4042,.T.);
#5304=ORIENTED_EDGE('',*,*,#4045,.F.);
#5305=ORIENTED_EDGE('',*,*,#4046,.T.);
#5306=ORIENTED_EDGE('',*,*,#4044,.T.);
#5307=ORIENTED_EDGE('',*,*,#4046,.F.);
#5308=ORIENTED_EDGE('',*,*,#4045,.T.);
#5309=ORIENTED_EDGE('',*,*,#4047,.F.);
#5310=ORIENTED_EDGE('',*,*,#4048,.F.);
#5311=ORIENTED_EDGE('',*,*,#4049,.T.);
#5312=ORIENTED_EDGE('',*,*,#4047,.T.);
#5313=ORIENTED_EDGE('',*,*,#4049,.F.);
#5314=ORIENTED_EDGE('',*,*,#4050,.F.);
#5315=ORIENTED_EDGE('',*,*,#4048,.T.);
#5316=ORIENTED_EDGE('',*,*,#4051,.F.);
#5317=ORIENTED_EDGE('',*,*,#4052,.T.);
#5318=ORIENTED_EDGE('',*,*,#4050,.T.);
#5319=ORIENTED_EDGE('',*,*,#4052,.F.);
#5320=ORIENTED_EDGE('',*,*,#4051,.T.);
#5321=ORIENTED_EDGE('',*,*,#4053,.F.);
#5322=ORIENTED_EDGE('',*,*,#4053,.T.);
#5323=ORIENTED_EDGE('',*,*,#4054,.T.);
#5324=ORIENTED_EDGE('',*,*,#4038,.F.);
#5325=ORIENTED_EDGE('',*,*,#4054,.F.);
#5326=ORIENTED_EDGE('',*,*,#4032,.T.);
#5327=ORIENTED_EDGE('',*,*,#4035,.T.);
#5328=ORIENTED_EDGE('',*,*,#4025,.T.);
#5329=ORIENTED_EDGE('',*,*,#4029,.T.);
#5330=ORIENTED_EDGE('',*,*,#4055,.F.);
#5331=ORIENTED_EDGE('',*,*,#4056,.F.);
#5332=ORIENTED_EDGE('',*,*,#4057,.F.);
#5333=ORIENTED_EDGE('',*,*,#4058,.F.);
#5334=ORIENTED_EDGE('',*,*,#4059,.F.);
#5335=ORIENTED_EDGE('',*,*,#4058,.T.);
#5336=ORIENTED_EDGE('',*,*,#4060,.F.);
#5337=ORIENTED_EDGE('',*,*,#4061,.T.);
#5338=ORIENTED_EDGE('',*,*,#4062,.F.);
#5339=ORIENTED_EDGE('',*,*,#4061,.F.);
#5340=ORIENTED_EDGE('',*,*,#4063,.F.);
#5341=ORIENTED_EDGE('',*,*,#4064,.F.);
#5342=ORIENTED_EDGE('',*,*,#4065,.F.);
#5343=ORIENTED_EDGE('',*,*,#4064,.T.);
#5344=ORIENTED_EDGE('',*,*,#4066,.F.);
#5345=ORIENTED_EDGE('',*,*,#4056,.T.);
#5346=ORIENTED_EDGE('',*,*,#4067,.F.);
#5347=ORIENTED_EDGE('',*,*,#4068,.T.);
#5348=ORIENTED_EDGE('',*,*,#4069,.F.);
#5349=ORIENTED_EDGE('',*,*,#4070,.T.);
#5350=ORIENTED_EDGE('',*,*,#4067,.T.);
#5351=ORIENTED_EDGE('',*,*,#4070,.F.);
#5352=ORIENTED_EDGE('',*,*,#4062,.T.);
#5353=ORIENTED_EDGE('',*,*,#4065,.T.);
#5354=ORIENTED_EDGE('',*,*,#4055,.T.);
#5355=ORIENTED_EDGE('',*,*,#4059,.T.);
#5356=ORIENTED_EDGE('',*,*,#4069,.T.);
#5357=ORIENTED_EDGE('',*,*,#4071,.F.);
#5358=ORIENTED_EDGE('',*,*,#4071,.T.);
#5359=ORIENTED_EDGE('',*,*,#4072,.T.);
#5360=ORIENTED_EDGE('',*,*,#4068,.F.);
#5361=ORIENTED_EDGE('',*,*,#4072,.F.);
#5362=ORIENTED_EDGE('',*,*,#4063,.T.);
#5363=ORIENTED_EDGE('',*,*,#4060,.T.);
#5364=ORIENTED_EDGE('',*,*,#4057,.T.);
#5365=ORIENTED_EDGE('',*,*,#4066,.T.);
#5366=ORIENTED_EDGE('',*,*,#4073,.T.);
#5367=ORIENTED_EDGE('',*,*,#4074,.T.);
#5368=ORIENTED_EDGE('',*,*,#4075,.T.);
#5369=ORIENTED_EDGE('',*,*,#4076,.F.);
#5370=ORIENTED_EDGE('',*,*,#4077,.T.);
#5371=ORIENTED_EDGE('',*,*,#4078,.T.);
#5372=ORIENTED_EDGE('',*,*,#4079,.T.);
#5373=ORIENTED_EDGE('',*,*,#4074,.F.);
#5374=ORIENTED_EDGE('',*,*,#4080,.T.);
#5375=ORIENTED_EDGE('',*,*,#4081,.T.);
#5376=ORIENTED_EDGE('',*,*,#4082,.T.);
#5377=ORIENTED_EDGE('',*,*,#4078,.F.);
#5378=ORIENTED_EDGE('',*,*,#4083,.T.);
#5379=ORIENTED_EDGE('',*,*,#4084,.T.);
#5380=ORIENTED_EDGE('',*,*,#4085,.T.);
#5381=ORIENTED_EDGE('',*,*,#4081,.F.);
#5382=ORIENTED_EDGE('',*,*,#4086,.T.);
#5383=ORIENTED_EDGE('',*,*,#4087,.T.);
#5384=ORIENTED_EDGE('',*,*,#4088,.T.);
#5385=ORIENTED_EDGE('',*,*,#4084,.F.);
#5386=ORIENTED_EDGE('',*,*,#4089,.T.);
#5387=ORIENTED_EDGE('',*,*,#4076,.T.);
#5388=ORIENTED_EDGE('',*,*,#4090,.T.);
#5389=ORIENTED_EDGE('',*,*,#4087,.F.);
#5390=ORIENTED_EDGE('',*,*,#4089,.F.);
#5391=ORIENTED_EDGE('',*,*,#4086,.F.);
#5392=ORIENTED_EDGE('',*,*,#4083,.F.);
#5393=ORIENTED_EDGE('',*,*,#4080,.F.);
#5394=ORIENTED_EDGE('',*,*,#4077,.F.);
#5395=ORIENTED_EDGE('',*,*,#4073,.F.);
#5396=ORIENTED_EDGE('',*,*,#4090,.F.);
#5397=ORIENTED_EDGE('',*,*,#4075,.F.);
#5398=ORIENTED_EDGE('',*,*,#4079,.F.);
#5399=ORIENTED_EDGE('',*,*,#4082,.F.);
#5400=ORIENTED_EDGE('',*,*,#4085,.F.);
#5401=ORIENTED_EDGE('',*,*,#4088,.F.);
#5402=ORIENTED_EDGE('',*,*,#4091,.F.);
#5403=ORIENTED_EDGE('',*,*,#4092,.F.);
#5404=ORIENTED_EDGE('',*,*,#4093,.F.);
#5405=ORIENTED_EDGE('',*,*,#4094,.T.);
#5406=ORIENTED_EDGE('',*,*,#4092,.T.);
#5407=ORIENTED_EDGE('',*,*,#4094,.F.);
#5408=ORIENTED_EDGE('',*,*,#4095,.F.);
#5409=ORIENTED_EDGE('',*,*,#4096,.T.);
#5410=ORIENTED_EDGE('',*,*,#4093,.T.);
#5411=ORIENTED_EDGE('',*,*,#4096,.F.);
#5412=ORIENTED_EDGE('',*,*,#4097,.F.);
#5413=ORIENTED_EDGE('',*,*,#4098,.T.);
#5414=ORIENTED_EDGE('',*,*,#4095,.T.);
#5415=ORIENTED_EDGE('',*,*,#4098,.F.);
#5416=ORIENTED_EDGE('',*,*,#4097,.T.);
#5417=ORIENTED_EDGE('',*,*,#4099,.F.);
#5418=ORIENTED_EDGE('',*,*,#4100,.F.);
#5419=ORIENTED_EDGE('',*,*,#4101,.T.);
#5420=ORIENTED_EDGE('',*,*,#4099,.T.);
#5421=ORIENTED_EDGE('',*,*,#4101,.F.);
#5422=ORIENTED_EDGE('',*,*,#4091,.T.);
#5423=ORIENTED_EDGE('',*,*,#4102,.T.);
#5424=ORIENTED_EDGE('',*,*,#4100,.T.);
#5425=ORIENTED_EDGE('',*,*,#4102,.F.);
#5426=ORIENTED_EDGE('',*,*,#4103,.F.);
#5427=ORIENTED_EDGE('',*,*,#4104,.T.);
#5428=ORIENTED_EDGE('',*,*,#4105,.F.);
#5429=ORIENTED_EDGE('',*,*,#4104,.F.);
#5430=ORIENTED_EDGE('',*,*,#4103,.T.);
#5431=ORIENTED_EDGE('',*,*,#4106,.F.);
#5432=ORIENTED_EDGE('',*,*,#4107,.T.);
#5433=ORIENTED_EDGE('',*,*,#4108,.T.);
#5434=ORIENTED_EDGE('',*,*,#4107,.F.);
#5435=ORIENTED_EDGE('',*,*,#4108,.F.);
#5436=ORIENTED_EDGE('',*,*,#4109,.F.);
#5437=ORIENTED_EDGE('',*,*,#4110,.T.);
#5438=ORIENTED_EDGE('',*,*,#4111,.F.);
#5439=ORIENTED_EDGE('',*,*,#4112,.T.);
#5440=ORIENTED_EDGE('',*,*,#4113,.F.);
#5441=ORIENTED_EDGE('',*,*,#4112,.F.);
#5442=ORIENTED_EDGE('',*,*,#4114,.F.);
#5443=ORIENTED_EDGE('',*,*,#4115,.F.);
#5444=ORIENTED_EDGE('',*,*,#4116,.F.);
#5445=ORIENTED_EDGE('',*,*,#4115,.T.);
#5446=ORIENTED_EDGE('',*,*,#4117,.T.);
#5447=ORIENTED_EDGE('',*,*,#4118,.T.);
#5448=ORIENTED_EDGE('',*,*,#4114,.T.);
#5449=ORIENTED_EDGE('',*,*,#4111,.T.);
#5450=ORIENTED_EDGE('',*,*,#4119,.T.);
#5451=ORIENTED_EDGE('',*,*,#4117,.F.);
#5452=ORIENTED_EDGE('',*,*,#4120,.F.);
#5453=ORIENTED_EDGE('',*,*,#4118,.F.);
#5454=ORIENTED_EDGE('',*,*,#4119,.F.);
#5455=ORIENTED_EDGE('',*,*,#4110,.F.);
#5456=ORIENTED_EDGE('',*,*,#4121,.F.);
#5457=ORIENTED_EDGE('',*,*,#4122,.T.);
#5458=ORIENTED_EDGE('',*,*,#4123,.F.);
#5459=ORIENTED_EDGE('',*,*,#4124,.T.);
#5460=ORIENTED_EDGE('',*,*,#4125,.F.);
#5461=ORIENTED_EDGE('',*,*,#4124,.F.);
#5462=ORIENTED_EDGE('',*,*,#4126,.F.);
#5463=ORIENTED_EDGE('',*,*,#4127,.F.);
#5464=ORIENTED_EDGE('',*,*,#4128,.F.);
#5465=ORIENTED_EDGE('',*,*,#4127,.T.);
#5466=ORIENTED_EDGE('',*,*,#4129,.T.);
#5467=ORIENTED_EDGE('',*,*,#4130,.T.);
#5468=ORIENTED_EDGE('',*,*,#4126,.T.);
#5469=ORIENTED_EDGE('',*,*,#4123,.T.);
#5470=ORIENTED_EDGE('',*,*,#4131,.T.);
#5471=ORIENTED_EDGE('',*,*,#4129,.F.);
#5472=ORIENTED_EDGE('',*,*,#4132,.F.);
#5473=ORIENTED_EDGE('',*,*,#4130,.F.);
#5474=ORIENTED_EDGE('',*,*,#4131,.F.);
#5475=ORIENTED_EDGE('',*,*,#4122,.F.);
#5476=ORIENTED_EDGE('',*,*,#4133,.F.);
#5477=ORIENTED_EDGE('',*,*,#4134,.T.);
#5478=ORIENTED_EDGE('',*,*,#4135,.T.);
#5479=ORIENTED_EDGE('',*,*,#4134,.F.);
#5480=ORIENTED_EDGE('',*,*,#4116,.T.);
#5481=ORIENTED_EDGE('',*,*,#4120,.T.);
#5482=ORIENTED_EDGE('',*,*,#4109,.T.);
#5483=ORIENTED_EDGE('',*,*,#4113,.T.);
#5484=ORIENTED_EDGE('',*,*,#4128,.T.);
#5485=ORIENTED_EDGE('',*,*,#4132,.T.);
#5486=ORIENTED_EDGE('',*,*,#4121,.T.);
#5487=ORIENTED_EDGE('',*,*,#4125,.T.);
#5488=ORIENTED_EDGE('',*,*,#4133,.T.);
#5489=ORIENTED_EDGE('',*,*,#4105,.T.);
#5490=ORIENTED_EDGE('',*,*,#4135,.F.);
#5491=ORIENTED_EDGE('',*,*,#4106,.T.);
#5492=ORIENTED_EDGE('',*,*,#4136,.F.);
#5493=ORIENTED_EDGE('',*,*,#4137,.T.);
#5494=ORIENTED_EDGE('',*,*,#4138,.T.);
#5495=ORIENTED_EDGE('',*,*,#4137,.F.);
#5496=ORIENTED_EDGE('',*,*,#4139,.F.);
#5497=ORIENTED_EDGE('',*,*,#4140,.T.);
#5498=ORIENTED_EDGE('',*,*,#4141,.T.);
#5499=ORIENTED_EDGE('',*,*,#4140,.F.);
#5500=ORIENTED_EDGE('',*,*,#4139,.T.);
#5501=ORIENTED_EDGE('',*,*,#4136,.T.);
#5502=ORIENTED_EDGE('',*,*,#4141,.F.);
#5503=ORIENTED_EDGE('',*,*,#4138,.F.);
#5504=ORIENTED_EDGE('',*,*,#4142,.F.);
#5505=ORIENTED_EDGE('',*,*,#4143,.T.);
#5506=ORIENTED_EDGE('',*,*,#4144,.T.);
#5507=ORIENTED_EDGE('',*,*,#4143,.F.);
#5508=ORIENTED_EDGE('',*,*,#4145,.F.);
#5509=ORIENTED_EDGE('',*,*,#4146,.T.);
#5510=ORIENTED_EDGE('',*,*,#4147,.T.);
#5511=ORIENTED_EDGE('',*,*,#4146,.F.);
#5512=ORIENTED_EDGE('',*,*,#4145,.T.);
#5513=ORIENTED_EDGE('',*,*,#4142,.T.);
#5514=ORIENTED_EDGE('',*,*,#4147,.F.);
#5515=ORIENTED_EDGE('',*,*,#4144,.F.);
#5516=ORIENTED_EDGE('',*,*,#4148,.F.);
#5517=ORIENTED_EDGE('',*,*,#4149,.T.);
#5518=ORIENTED_EDGE('',*,*,#4150,.T.);
#5519=ORIENTED_EDGE('',*,*,#4149,.F.);
#5520=ORIENTED_EDGE('',*,*,#4151,.F.);
#5521=ORIENTED_EDGE('',*,*,#4152,.T.);
#5522=ORIENTED_EDGE('',*,*,#4153,.T.);
#5523=ORIENTED_EDGE('',*,*,#4152,.F.);
#5524=ORIENTED_EDGE('',*,*,#4151,.T.);
#5525=ORIENTED_EDGE('',*,*,#4148,.T.);
#5526=ORIENTED_EDGE('',*,*,#4153,.F.);
#5527=ORIENTED_EDGE('',*,*,#4150,.F.);
#5528=ORIENTED_EDGE('',*,*,#4154,.F.);
#5529=ORIENTED_EDGE('',*,*,#4155,.T.);
#5530=ORIENTED_EDGE('',*,*,#4156,.T.);
#5531=ORIENTED_EDGE('',*,*,#4155,.F.);
#5532=ORIENTED_EDGE('',*,*,#4157,.F.);
#5533=ORIENTED_EDGE('',*,*,#4158,.T.);
#5534=ORIENTED_EDGE('',*,*,#4159,.T.);
#5535=ORIENTED_EDGE('',*,*,#4158,.F.);
#5536=ORIENTED_EDGE('',*,*,#4157,.T.);
#5537=ORIENTED_EDGE('',*,*,#4154,.T.);
#5538=ORIENTED_EDGE('',*,*,#4159,.F.);
#5539=ORIENTED_EDGE('',*,*,#4156,.F.);
#5540=ORIENTED_EDGE('',*,*,#4160,.F.);
#5541=ORIENTED_EDGE('',*,*,#4161,.T.);
#5542=ORIENTED_EDGE('',*,*,#4162,.F.);
#5543=ORIENTED_EDGE('',*,*,#4163,.F.);
#5544=ORIENTED_EDGE('',*,*,#4164,.F.);
#5545=ORIENTED_EDGE('',*,*,#4165,.T.);
#5546=ORIENTED_EDGE('',*,*,#4166,.F.);
#5547=ORIENTED_EDGE('',*,*,#4161,.F.);
#5548=ORIENTED_EDGE('',*,*,#4167,.F.);
#5549=ORIENTED_EDGE('',*,*,#4168,.F.);
#5550=ORIENTED_EDGE('',*,*,#4169,.F.);
#5551=ORIENTED_EDGE('',*,*,#4165,.F.);
#5552=ORIENTED_EDGE('',*,*,#4170,.T.);
#5553=ORIENTED_EDGE('',*,*,#4162,.T.);
#5554=ORIENTED_EDGE('',*,*,#4166,.T.);
#5555=ORIENTED_EDGE('',*,*,#4169,.T.);
#5556=ORIENTED_EDGE('',*,*,#4171,.T.);
#5557=ORIENTED_EDGE('',*,*,#4163,.T.);
#5558=ORIENTED_EDGE('',*,*,#4171,.F.);
#5559=ORIENTED_EDGE('',*,*,#4168,.T.);
#5560=ORIENTED_EDGE('',*,*,#4172,.F.);
#5561=ORIENTED_EDGE('',*,*,#4173,.F.);
#5562=ORIENTED_EDGE('',*,*,#4174,.T.);
#5563=ORIENTED_EDGE('',*,*,#4175,.T.);
#5564=ORIENTED_EDGE('',*,*,#4174,.F.);
#5565=ORIENTED_EDGE('',*,*,#4170,.F.);
#5566=ORIENTED_EDGE('',*,*,#4176,.T.);
#5567=ORIENTED_EDGE('',*,*,#4177,.F.);
#5568=ORIENTED_EDGE('',*,*,#4176,.F.);
#5569=ORIENTED_EDGE('',*,*,#4175,.F.);
#5570=ORIENTED_EDGE('',*,*,#4160,.T.);
#5571=ORIENTED_EDGE('',*,*,#4172,.T.);
#5572=ORIENTED_EDGE('',*,*,#4167,.T.);
#5573=ORIENTED_EDGE('',*,*,#4164,.T.);
#5574=ORIENTED_EDGE('',*,*,#4178,.F.);
#5575=ORIENTED_EDGE('',*,*,#4179,.T.);
#5576=ORIENTED_EDGE('',*,*,#4180,.T.);
#5577=ORIENTED_EDGE('',*,*,#4179,.F.);
#5578=ORIENTED_EDGE('',*,*,#4178,.T.);
#5579=ORIENTED_EDGE('',*,*,#4177,.T.);
#5580=ORIENTED_EDGE('',*,*,#4180,.F.);
#5581=ORIENTED_EDGE('',*,*,#4173,.T.);
#5582=ORIENTED_EDGE('',*,*,#4181,.F.);
#5583=ORIENTED_EDGE('',*,*,#4182,.T.);
#5584=ORIENTED_EDGE('',*,*,#4183,.F.);
#5585=ORIENTED_EDGE('',*,*,#4182,.F.);
#5586=ORIENTED_EDGE('',*,*,#4184,.F.);
#5587=ORIENTED_EDGE('',*,*,#4185,.T.);
#5588=ORIENTED_EDGE('',*,*,#4186,.F.);
#5589=ORIENTED_EDGE('',*,*,#4187,.F.);
#5590=ORIENTED_EDGE('',*,*,#4188,.F.);
#5591=ORIENTED_EDGE('',*,*,#4189,.T.);
#5592=ORIENTED_EDGE('',*,*,#4190,.F.);
#5593=ORIENTED_EDGE('',*,*,#4185,.F.);
#5594=ORIENTED_EDGE('',*,*,#4191,.F.);
#5595=ORIENTED_EDGE('',*,*,#4192,.F.);
#5596=ORIENTED_EDGE('',*,*,#4193,.F.);
#5597=ORIENTED_EDGE('',*,*,#4189,.F.);
#5598=ORIENTED_EDGE('',*,*,#4194,.T.);
#5599=ORIENTED_EDGE('',*,*,#4186,.T.);
#5600=ORIENTED_EDGE('',*,*,#4190,.T.);
#5601=ORIENTED_EDGE('',*,*,#4193,.T.);
#5602=ORIENTED_EDGE('',*,*,#4195,.T.);
#5603=ORIENTED_EDGE('',*,*,#4187,.T.);
#5604=ORIENTED_EDGE('',*,*,#4195,.F.);
#5605=ORIENTED_EDGE('',*,*,#4192,.T.);
#5606=ORIENTED_EDGE('',*,*,#4196,.T.);
#5607=ORIENTED_EDGE('',*,*,#4197,.F.);
#5608=ORIENTED_EDGE('',*,*,#4198,.F.);
#5609=ORIENTED_EDGE('',*,*,#4199,.F.);
#5610=ORIENTED_EDGE('',*,*,#4200,.T.);
#5611=ORIENTED_EDGE('',*,*,#4200,.F.);
#5612=ORIENTED_EDGE('',*,*,#4201,.T.);
#5613=ORIENTED_EDGE('',*,*,#4202,.F.);
#5614=ORIENTED_EDGE('',*,*,#4203,.T.);
#5615=ORIENTED_EDGE('',*,*,#4181,.T.);
#5616=ORIENTED_EDGE('',*,*,#4199,.T.);
#5617=ORIENTED_EDGE('',*,*,#4204,.F.);
#5618=ORIENTED_EDGE('',*,*,#4205,.F.);
#5619=ORIENTED_EDGE('',*,*,#4201,.F.);
#5620=ORIENTED_EDGE('',*,*,#4197,.T.);
#5621=ORIENTED_EDGE('',*,*,#4203,.F.);
#5622=ORIENTED_EDGE('',*,*,#4206,.F.);
#5623=ORIENTED_EDGE('',*,*,#4207,.F.);
#5624=ORIENTED_EDGE('',*,*,#4207,.T.);
#5625=ORIENTED_EDGE('',*,*,#4208,.F.);
#5626=ORIENTED_EDGE('',*,*,#4204,.T.);
#5627=ORIENTED_EDGE('',*,*,#4198,.T.);
#5628=ORIENTED_EDGE('',*,*,#4183,.T.);
#5629=ORIENTED_EDGE('',*,*,#4194,.F.);
#5630=ORIENTED_EDGE('',*,*,#4209,.T.);
#5631=ORIENTED_EDGE('',*,*,#4210,.T.);
#5632=ORIENTED_EDGE('',*,*,#4209,.F.);
#5633=ORIENTED_EDGE('',*,*,#4205,.T.);
#5634=ORIENTED_EDGE('',*,*,#4208,.T.);
#5635=ORIENTED_EDGE('',*,*,#4206,.T.);
#5636=ORIENTED_EDGE('',*,*,#4202,.T.);
#5637=ORIENTED_EDGE('',*,*,#4210,.F.);
#5638=ORIENTED_EDGE('',*,*,#4184,.T.);
#5639=ORIENTED_EDGE('',*,*,#4196,.F.);
#5640=ORIENTED_EDGE('',*,*,#4191,.T.);
#5641=ORIENTED_EDGE('',*,*,#4188,.T.);
#5642=ORIENTED_EDGE('',*,*,#4211,.F.);
#5643=ORIENTED_EDGE('',*,*,#4212,.T.);
#5644=ORIENTED_EDGE('',*,*,#4213,.T.);
#5645=ORIENTED_EDGE('',*,*,#4212,.F.);
#5646=ORIENTED_EDGE('',*,*,#4213,.F.);
#5647=ORIENTED_EDGE('',*,*,#4214,.F.);
#5648=ORIENTED_EDGE('',*,*,#4215,.T.);
#5649=ORIENTED_EDGE('',*,*,#4216,.T.);
#5650=ORIENTED_EDGE('',*,*,#4215,.F.);
#5651=ORIENTED_EDGE('',*,*,#4214,.T.);
#5652=ORIENTED_EDGE('',*,*,#4216,.F.);
#5653=ORIENTED_EDGE('',*,*,#4211,.T.);
#5654=ORIENTED_EDGE('',*,*,#4217,.F.);
#5655=ORIENTED_EDGE('',*,*,#4218,.T.);
#5656=ORIENTED_EDGE('',*,*,#4219,.T.);
#5657=ORIENTED_EDGE('',*,*,#4218,.F.);
#5658=ORIENTED_EDGE('',*,*,#4220,.F.);
#5659=ORIENTED_EDGE('',*,*,#4221,.T.);
#5660=ORIENTED_EDGE('',*,*,#4222,.T.);
#5661=ORIENTED_EDGE('',*,*,#4221,.F.);
#5662=ORIENTED_EDGE('',*,*,#4220,.T.);
#5663=ORIENTED_EDGE('',*,*,#4217,.T.);
#5664=ORIENTED_EDGE('',*,*,#4222,.F.);
#5665=ORIENTED_EDGE('',*,*,#4219,.F.);
#5666=ORIENTED_EDGE('',*,*,#4223,.F.);
#5667=ORIENTED_EDGE('',*,*,#4224,.T.);
#5668=ORIENTED_EDGE('',*,*,#4225,.T.);
#5669=ORIENTED_EDGE('',*,*,#4224,.F.);
#5670=ORIENTED_EDGE('',*,*,#4226,.F.);
#5671=ORIENTED_EDGE('',*,*,#4227,.T.);
#5672=ORIENTED_EDGE('',*,*,#4228,.T.);
#5673=ORIENTED_EDGE('',*,*,#4227,.F.);
#5674=ORIENTED_EDGE('',*,*,#4226,.T.);
#5675=ORIENTED_EDGE('',*,*,#4223,.T.);
#5676=ORIENTED_EDGE('',*,*,#4228,.F.);
#5677=ORIENTED_EDGE('',*,*,#4225,.F.);
#5678=ORIENTED_EDGE('',*,*,#4229,.F.);
#5679=ORIENTED_EDGE('',*,*,#4230,.F.);
#5680=ORIENTED_EDGE('',*,*,#4231,.F.);
#5681=ORIENTED_EDGE('',*,*,#4232,.F.);
#5682=ORIENTED_EDGE('',*,*,#4233,.F.);
#5683=ORIENTED_EDGE('',*,*,#4234,.F.);
#5684=ORIENTED_EDGE('',*,*,#4235,.F.);
#5685=ORIENTED_EDGE('',*,*,#4236,.F.);
#5686=ORIENTED_EDGE('',*,*,#4233,.T.);
#5687=ORIENTED_EDGE('',*,*,#4237,.T.);
#5688=ORIENTED_EDGE('',*,*,#4238,.T.);
#5689=ORIENTED_EDGE('',*,*,#4239,.T.);
#5690=ORIENTED_EDGE('',*,*,#4232,.T.);
#5691=ORIENTED_EDGE('',*,*,#4240,.F.);
#5692=ORIENTED_EDGE('',*,*,#4241,.T.);
#5693=ORIENTED_EDGE('',*,*,#4237,.F.);
#5694=ORIENTED_EDGE('',*,*,#4231,.T.);
#5695=ORIENTED_EDGE('',*,*,#4242,.T.);
#5696=ORIENTED_EDGE('',*,*,#4243,.T.);
#5697=ORIENTED_EDGE('',*,*,#4240,.T.);
#5698=ORIENTED_EDGE('',*,*,#4230,.T.);
#5699=ORIENTED_EDGE('',*,*,#4244,.F.);
#5700=ORIENTED_EDGE('',*,*,#4245,.T.);
#5701=ORIENTED_EDGE('',*,*,#4242,.F.);
#5702=ORIENTED_EDGE('',*,*,#4238,.F.);
#5703=ORIENTED_EDGE('',*,*,#4241,.F.);
#5704=ORIENTED_EDGE('',*,*,#4243,.F.);
#5705=ORIENTED_EDGE('',*,*,#4245,.F.);
#5706=ORIENTED_EDGE('',*,*,#4246,.F.);
#5707=ORIENTED_EDGE('',*,*,#4247,.F.);
#5708=ORIENTED_EDGE('',*,*,#4248,.F.);
#5709=ORIENTED_EDGE('',*,*,#4249,.F.);
#5710=ORIENTED_EDGE('',*,*,#4229,.T.);
#5711=ORIENTED_EDGE('',*,*,#4250,.T.);
#5712=ORIENTED_EDGE('',*,*,#4246,.T.);
#5713=ORIENTED_EDGE('',*,*,#4244,.T.);
#5714=ORIENTED_EDGE('',*,*,#4236,.T.);
#5715=ORIENTED_EDGE('',*,*,#4251,.F.);
#5716=ORIENTED_EDGE('',*,*,#4247,.T.);
#5717=ORIENTED_EDGE('',*,*,#4250,.F.);
#5718=ORIENTED_EDGE('',*,*,#4235,.T.);
#5719=ORIENTED_EDGE('',*,*,#4252,.T.);
#5720=ORIENTED_EDGE('',*,*,#4248,.T.);
#5721=ORIENTED_EDGE('',*,*,#4251,.T.);
#5722=ORIENTED_EDGE('',*,*,#4234,.T.);
#5723=ORIENTED_EDGE('',*,*,#4239,.F.);
#5724=ORIENTED_EDGE('',*,*,#4249,.T.);
#5725=ORIENTED_EDGE('',*,*,#4252,.F.);
#5726=ORIENTED_EDGE('',*,*,#4253,.F.);
#5727=ORIENTED_EDGE('',*,*,#4254,.F.);
#5728=ORIENTED_EDGE('',*,*,#4255,.T.);
#5729=ORIENTED_EDGE('',*,*,#4253,.T.);
#5730=ORIENTED_EDGE('',*,*,#4255,.F.);
#5731=ORIENTED_EDGE('',*,*,#4256,.F.);
#5732=ORIENTED_EDGE('',*,*,#4257,.T.);
#5733=ORIENTED_EDGE('',*,*,#4254,.T.);
#5734=ORIENTED_EDGE('',*,*,#4257,.F.);
#5735=ORIENTED_EDGE('',*,*,#4258,.F.);
#5736=ORIENTED_EDGE('',*,*,#4259,.T.);
#5737=ORIENTED_EDGE('',*,*,#4256,.T.);
#5738=ORIENTED_EDGE('',*,*,#4259,.F.);
#5739=ORIENTED_EDGE('',*,*,#4258,.T.);
#5740=ORIENTED_EDGE('',*,*,#4260,.F.);
#5741=ORIENTED_EDGE('',*,*,#4261,.F.);
#5742=ORIENTED_EDGE('',*,*,#4262,.T.);
#5743=ORIENTED_EDGE('',*,*,#4260,.T.);
#5744=ORIENTED_EDGE('',*,*,#4262,.F.);
#5745=ORIENTED_EDGE('',*,*,#4263,.F.);
#5746=ORIENTED_EDGE('',*,*,#4264,.T.);
#5747=ORIENTED_EDGE('',*,*,#4261,.T.);
#5748=ORIENTED_EDGE('',*,*,#4264,.F.);
#5749=ORIENTED_EDGE('',*,*,#4265,.F.);
#5750=ORIENTED_EDGE('',*,*,#4266,.T.);
#5751=ORIENTED_EDGE('',*,*,#4263,.T.);
#5752=ORIENTED_EDGE('',*,*,#4266,.F.);
#5753=ORIENTED_EDGE('',*,*,#4265,.T.);
#5754=ORIENTED_EDGE('',*,*,#4267,.T.);
#5755=ORIENTED_EDGE('',*,*,#4268,.T.);
#5756=ORIENTED_EDGE('',*,*,#4269,.T.);
#5757=ORIENTED_EDGE('',*,*,#4270,.F.);
#5758=ORIENTED_EDGE('',*,*,#4271,.T.);
#5759=ORIENTED_EDGE('',*,*,#4272,.T.);
#5760=ORIENTED_EDGE('',*,*,#4273,.T.);
#5761=ORIENTED_EDGE('',*,*,#4268,.F.);
#5762=ORIENTED_EDGE('',*,*,#4274,.T.);
#5763=ORIENTED_EDGE('',*,*,#4275,.T.);
#5764=ORIENTED_EDGE('',*,*,#4276,.T.);
#5765=ORIENTED_EDGE('',*,*,#4272,.F.);
#5766=ORIENTED_EDGE('',*,*,#4277,.T.);
#5767=ORIENTED_EDGE('',*,*,#4278,.T.);
#5768=ORIENTED_EDGE('',*,*,#4279,.T.);
#5769=ORIENTED_EDGE('',*,*,#4275,.F.);
#5770=ORIENTED_EDGE('',*,*,#4280,.T.);
#5771=ORIENTED_EDGE('',*,*,#4281,.T.);
#5772=ORIENTED_EDGE('',*,*,#4282,.T.);
#5773=ORIENTED_EDGE('',*,*,#4278,.F.);
#5774=ORIENTED_EDGE('',*,*,#4283,.T.);
#5775=ORIENTED_EDGE('',*,*,#4270,.T.);
#5776=ORIENTED_EDGE('',*,*,#4284,.T.);
#5777=ORIENTED_EDGE('',*,*,#4281,.F.);
#5778=ORIENTED_EDGE('',*,*,#4283,.F.);
#5779=ORIENTED_EDGE('',*,*,#4280,.F.);
#5780=ORIENTED_EDGE('',*,*,#4277,.F.);
#5781=ORIENTED_EDGE('',*,*,#4274,.F.);
#5782=ORIENTED_EDGE('',*,*,#4271,.F.);
#5783=ORIENTED_EDGE('',*,*,#4267,.F.);
#5784=ORIENTED_EDGE('',*,*,#4284,.F.);
#5785=ORIENTED_EDGE('',*,*,#4269,.F.);
#5786=ORIENTED_EDGE('',*,*,#4273,.F.);
#5787=ORIENTED_EDGE('',*,*,#4276,.F.);
#5788=ORIENTED_EDGE('',*,*,#4279,.F.);
#5789=ORIENTED_EDGE('',*,*,#4282,.F.);
#5790=ORIENTED_EDGE('',*,*,#4285,.F.);
#5791=ORIENTED_EDGE('',*,*,#4286,.T.);
#5792=ORIENTED_EDGE('',*,*,#4287,.F.);
#5793=ORIENTED_EDGE('',*,*,#4286,.F.);
#5794=ORIENTED_EDGE('',*,*,#4288,.T.);
#5795=ORIENTED_EDGE('',*,*,#4289,.T.);
#5796=ORIENTED_EDGE('',*,*,#4290,.F.);
#5797=ORIENTED_EDGE('',*,*,#4291,.F.);
#5798=ORIENTED_EDGE('',*,*,#4292,.T.);
#5799=ORIENTED_EDGE('',*,*,#4291,.T.);
#5800=ORIENTED_EDGE('',*,*,#4293,.F.);
#5801=ORIENTED_EDGE('',*,*,#4294,.F.);
#5802=ORIENTED_EDGE('',*,*,#4295,.T.);
#5803=ORIENTED_EDGE('',*,*,#4294,.T.);
#5804=ORIENTED_EDGE('',*,*,#4296,.F.);
#5805=ORIENTED_EDGE('',*,*,#4297,.F.);
#5806=ORIENTED_EDGE('',*,*,#4298,.T.);
#5807=ORIENTED_EDGE('',*,*,#4297,.T.);
#5808=ORIENTED_EDGE('',*,*,#4299,.F.);
#5809=ORIENTED_EDGE('',*,*,#4289,.F.);
#5810=ORIENTED_EDGE('',*,*,#4299,.T.);
#5811=ORIENTED_EDGE('',*,*,#4296,.T.);
#5812=ORIENTED_EDGE('',*,*,#4293,.T.);
#5813=ORIENTED_EDGE('',*,*,#4290,.T.);
#5814=ORIENTED_EDGE('',*,*,#4287,.T.);
#5815=ORIENTED_EDGE('',*,*,#4298,.F.);
#5816=ORIENTED_EDGE('',*,*,#4288,.F.);
#5817=ORIENTED_EDGE('',*,*,#4292,.F.);
#5818=ORIENTED_EDGE('',*,*,#4295,.F.);
#5819=ORIENTED_EDGE('',*,*,#4285,.T.);
#5820=ORIENTED_EDGE('',*,*,#4300,.F.);
#5821=ORIENTED_EDGE('',*,*,#4301,.T.);
#5822=ORIENTED_EDGE('',*,*,#4302,.F.);
#5823=ORIENTED_EDGE('',*,*,#4301,.F.);
#5824=ORIENTED_EDGE('',*,*,#4303,.F.);
#5825=ORIENTED_EDGE('',*,*,#4304,.T.);
#5826=ORIENTED_EDGE('',*,*,#4305,.F.);
#5827=ORIENTED_EDGE('',*,*,#4304,.F.);
#5828=ORIENTED_EDGE('',*,*,#4306,.F.);
#5829=ORIENTED_EDGE('',*,*,#4307,.T.);
#5830=ORIENTED_EDGE('',*,*,#4308,.F.);
#5831=ORIENTED_EDGE('',*,*,#4307,.F.);
#5832=ORIENTED_EDGE('',*,*,#4309,.F.);
#5833=ORIENTED_EDGE('',*,*,#4310,.T.);
#5834=ORIENTED_EDGE('',*,*,#4311,.F.);
#5835=ORIENTED_EDGE('',*,*,#4310,.F.);
#5836=ORIENTED_EDGE('',*,*,#4312,.F.);
#5837=ORIENTED_EDGE('',*,*,#4313,.F.);
#5838=ORIENTED_EDGE('',*,*,#4314,.F.);
#5839=ORIENTED_EDGE('',*,*,#4315,.F.);
#5840=ORIENTED_EDGE('',*,*,#4316,.T.);
#5841=ORIENTED_EDGE('',*,*,#4309,.T.);
#5842=ORIENTED_EDGE('',*,*,#4306,.T.);
#5843=ORIENTED_EDGE('',*,*,#4303,.T.);
#5844=ORIENTED_EDGE('',*,*,#4300,.T.);
#5845=ORIENTED_EDGE('',*,*,#4313,.T.);
#5846=ORIENTED_EDGE('',*,*,#4317,.T.);
#5847=ORIENTED_EDGE('',*,*,#4318,.F.);
#5848=ORIENTED_EDGE('',*,*,#4319,.F.);
#5849=ORIENTED_EDGE('',*,*,#4314,.T.);
#5850=ORIENTED_EDGE('',*,*,#4319,.T.);
#5851=ORIENTED_EDGE('',*,*,#4320,.F.);
#5852=ORIENTED_EDGE('',*,*,#4321,.F.);
#5853=ORIENTED_EDGE('',*,*,#4315,.T.);
#5854=ORIENTED_EDGE('',*,*,#4321,.T.);
#5855=ORIENTED_EDGE('',*,*,#4322,.F.);
#5856=ORIENTED_EDGE('',*,*,#4323,.F.);
#5857=ORIENTED_EDGE('',*,*,#4312,.T.);
#5858=ORIENTED_EDGE('',*,*,#4323,.T.);
#5859=ORIENTED_EDGE('',*,*,#4324,.F.);
#5860=ORIENTED_EDGE('',*,*,#4317,.F.);
#5861=ORIENTED_EDGE('',*,*,#4324,.T.);
#5862=ORIENTED_EDGE('',*,*,#4322,.T.);
#5863=ORIENTED_EDGE('',*,*,#4320,.T.);
#5864=ORIENTED_EDGE('',*,*,#4318,.T.);
#5865=ORIENTED_EDGE('',*,*,#4302,.T.);
#5866=ORIENTED_EDGE('',*,*,#4305,.T.);
#5867=ORIENTED_EDGE('',*,*,#4308,.T.);
#5868=ORIENTED_EDGE('',*,*,#4311,.T.);
#5869=ORIENTED_EDGE('',*,*,#4325,.F.);
#5870=ORIENTED_EDGE('',*,*,#4326,.T.);
#5871=ORIENTED_EDGE('',*,*,#4327,.T.);
#5872=ORIENTED_EDGE('',*,*,#4326,.F.);
#5873=ORIENTED_EDGE('',*,*,#4327,.F.);
#5874=ORIENTED_EDGE('',*,*,#4316,.F.);
#5875=ORIENTED_EDGE('',*,*,#4328,.T.);
#5876=ORIENTED_EDGE('',*,*,#4329,.T.);
#5877=ORIENTED_EDGE('',*,*,#4328,.F.);
#5878=ORIENTED_EDGE('',*,*,#4329,.F.);
#5879=ORIENTED_EDGE('',*,*,#4325,.T.);
#5880=ORIENTED_EDGE('',*,*,#4330,.F.);
#5881=ORIENTED_EDGE('',*,*,#4331,.T.);
#5882=ORIENTED_EDGE('',*,*,#4332,.T.);
#5883=ORIENTED_EDGE('',*,*,#4331,.F.);
#5884=ORIENTED_EDGE('',*,*,#4333,.F.);
#5885=ORIENTED_EDGE('',*,*,#4334,.T.);
#5886=ORIENTED_EDGE('',*,*,#4335,.T.);
#5887=ORIENTED_EDGE('',*,*,#4334,.F.);
#5888=ORIENTED_EDGE('',*,*,#4333,.T.);
#5889=ORIENTED_EDGE('',*,*,#4330,.T.);
#5890=ORIENTED_EDGE('',*,*,#4335,.F.);
#5891=ORIENTED_EDGE('',*,*,#4332,.F.);
#5892=CYLINDRICAL_SURFACE('',#6856,0.21);
#5893=CYLINDRICAL_SURFACE('',#6859,0.21);
#5894=CYLINDRICAL_SURFACE('',#6862,0.165);
#5895=CYLINDRICAL_SURFACE('',#6865,0.165);
#5896=CYLINDRICAL_SURFACE('',#6868,0.165);
#5897=CYLINDRICAL_SURFACE('',#6871,0.165);
#5898=CYLINDRICAL_SURFACE('',#6900,0.225);
#5899=CYLINDRICAL_SURFACE('',#6903,0.225);
#5900=CYLINDRICAL_SURFACE('',#6906,0.165);
#5901=CYLINDRICAL_SURFACE('',#6909,0.165);
#5902=CYLINDRICAL_SURFACE('',#6912,0.165);
#5903=CYLINDRICAL_SURFACE('',#6915,0.165);
#5904=CYLINDRICAL_SURFACE('',#6918,1.6);
#5905=CYLINDRICAL_SURFACE('',#6932,0.225);
#5906=CYLINDRICAL_SURFACE('',#6935,0.225);
#5907=CYLINDRICAL_SURFACE('',#6938,0.225);
#5908=CYLINDRICAL_SURFACE('',#6941,0.225);
#5909=CYLINDRICAL_SURFACE('',#6944,1.59);
#5910=CYLINDRICAL_SURFACE('',#6949,1.005);
#5911=CYLINDRICAL_SURFACE('',#6951,2.4);
#5912=CYLINDRICAL_SURFACE('',#6957,0.225);
#5913=CYLINDRICAL_SURFACE('',#6960,0.225);
#5914=CYLINDRICAL_SURFACE('',#6963,0.225);
#5915=CYLINDRICAL_SURFACE('',#6966,0.225);
#5916=CYLINDRICAL_SURFACE('',#6969,1.59);
#5917=CYLINDRICAL_SURFACE('',#6974,1.005);
#5918=CYLINDRICAL_SURFACE('',#6976,2.4);
#5919=CYLINDRICAL_SURFACE('',#6982,0.225);
#5920=CYLINDRICAL_SURFACE('',#6985,0.225);
#5921=CYLINDRICAL_SURFACE('',#6988,0.165);
#5922=CYLINDRICAL_SURFACE('',#6991,0.165);
#5923=CYLINDRICAL_SURFACE('',#6994,0.165);
#5924=CYLINDRICAL_SURFACE('',#6997,0.165);
#5925=CYLINDRICAL_SURFACE('',#7000,1.6);
#5926=CYLINDRICAL_SURFACE('',#7014,0.225);
#5927=CYLINDRICAL_SURFACE('',#7017,0.225);
#5928=CYLINDRICAL_SURFACE('',#7020,0.225);
#5929=CYLINDRICAL_SURFACE('',#7023,0.225);
#5930=CYLINDRICAL_SURFACE('',#7026,1.59);
#5931=CYLINDRICAL_SURFACE('',#7031,1.005);
#5932=CYLINDRICAL_SURFACE('',#7033,2.4);
#5933=CYLINDRICAL_SURFACE('',#7039,0.225);
#5934=CYLINDRICAL_SURFACE('',#7042,0.225);
#5935=CYLINDRICAL_SURFACE('',#7045,0.225);
#5936=CYLINDRICAL_SURFACE('',#7048,0.225);
#5937=CYLINDRICAL_SURFACE('',#7051,1.59);
#5938=CYLINDRICAL_SURFACE('',#7056,1.005);
#5939=CYLINDRICAL_SURFACE('',#7058,2.4);
#5940=CYLINDRICAL_SURFACE('',#7064,0.165);
#5941=CYLINDRICAL_SURFACE('',#7068,0.165);
#5942=CYLINDRICAL_SURFACE('',#7072,0.165);
#5943=CYLINDRICAL_SURFACE('',#7076,0.165);
#5944=CYLINDRICAL_SURFACE('',#7080,1.05);
#5945=CYLINDRICAL_SURFACE('',#7085,0.625);
#5946=CYLINDRICAL_SURFACE('',#7087,0.5);
#5947=CYLINDRICAL_SURFACE('',#7092,0.275);
#5948=CYLINDRICAL_SURFACE('',#7094,0.5);
#5949=CYLINDRICAL_SURFACE('',#7099,0.275);
#5950=CYLINDRICAL_SURFACE('',#7116,0.625);
#5951=CYLINDRICAL_SURFACE('',#7119,1.04);
#5952=CYLINDRICAL_SURFACE('',#7125,0.225);
#5953=CYLINDRICAL_SURFACE('',#7128,0.225);
#5954=CYLINDRICAL_SURFACE('',#7131,0.225);
#5955=CYLINDRICAL_SURFACE('',#7134,0.225);
#5956=CYLINDRICAL_SURFACE('',#7137,1.04);
#5957=CYLINDRICAL_SURFACE('',#7142,0.625);
#5958=CYLINDRICAL_SURFACE('',#7144,1.8);
#5959=CYLINDRICAL_SURFACE('',#7162,1.070235);
#5960=CYLINDRICAL_SURFACE('',#7164,0.6);
#5961=CYLINDRICAL_SURFACE('',#7170,1.070235);
#5962=CYLINDRICAL_SURFACE('',#7182,1.129765);
#5963=CYLINDRICAL_SURFACE('',#7189,1.6);
#5964=CYLINDRICAL_SURFACE('',#7194,1.129765);
#5965=CYLINDRICAL_SURFACE('',#7214,1.123812);
#5966=CYLINDRICAL_SURFACE('',#7250,1.076188);
#5967=CYLINDRICAL_SURFACE('',#7264,1.119765);
#5968=CYLINDRICAL_SURFACE('',#7268,1.085235);
#5969=CYLINDRICAL_SURFACE('',#7272,1.119765);
#5970=CYLINDRICAL_SURFACE('',#7276,1.085235);
#5971=CYLINDRICAL_SURFACE('',#7287,0.425);
#5972=CYLINDRICAL_SURFACE('',#7295,0.24505);
#5973=CYLINDRICAL_SURFACE('',#7320,1.05);
#5974=CYLINDRICAL_SURFACE('',#7324,1.);
#5975=CYLINDRICAL_SURFACE('',#7328,1.05);
#5976=CYLINDRICAL_SURFACE('',#7332,1.);
#5977=CYLINDRICAL_SURFACE('',#7336,1.05);
#5978=CYLINDRICAL_SURFACE('',#7340,0.9);
#5979=CYLINDRICAL_SURFACE('',#7353,0.895);
#5980=CYLINDRICAL_SURFACE('',#7357,0.605);
#5981=CYLINDRICAL_SURFACE('',#7375,0.35);
#5982=CYLINDRICAL_SURFACE('',#7383,0.1954);
#5983=CYLINDRICAL_SURFACE('',#7386,0.165);
#5984=CYLINDRICAL_SURFACE('',#7390,0.165);
#5985=CYLINDRICAL_SURFACE('',#7408,0.6);
#5986=CYLINDRICAL_SURFACE('',#7414,0.605);
#5987=CYLINDRICAL_SURFACE('',#7417,0.8);
#5988=CYLINDRICAL_SURFACE('',#7423,0.605);
#5989=CYLINDRICAL_SURFACE('',#7426,0.8);
#5990=CYLINDRICAL_SURFACE('',#7432,0.605);
#5991=CYLINDRICAL_SURFACE('',#7435,0.8);
#5992=CYLINDRICAL_SURFACE('',#7441,0.605);
#5993=CYLINDRICAL_SURFACE('',#7444,0.8);
#5994=CYLINDRICAL_SURFACE('',#7456,0.6);
#5995=CYLINDRICAL_SURFACE('',#7458,0.9);
#5996=CYLINDRICAL_SURFACE('',#7461,0.9);
#5997=CYLINDRICAL_SURFACE('',#7464,2.);
#5998=CYLINDRICAL_SURFACE('',#7470,0.225);
#5999=CYLINDRICAL_SURFACE('',#7479,0.6);
#6000=CYLINDRICAL_SURFACE('',#7481,0.7);
#6001=CYLINDRICAL_SURFACE('',#7490,1.2);
#6002=CYLINDRICAL_SURFACE('',#7494,0.165);
#6003=CYLINDRICAL_SURFACE('',#7498,0.6);
#6004=CYLINDRICAL_SURFACE('',#7504,0.225);
#6005=CYLINDRICAL_SURFACE('',#7507,1.);
#6006=CYLINDRICAL_SURFACE('',#7513,0.225);
#6007=CYLINDRICAL_SURFACE('',#7516,1.);
#6008=CYLINDRICAL_SURFACE('',#7537,0.35);
#6009=CYLINDRICAL_SURFACE('',#7545,0.1954);
#6010=CYLINDRICAL_SURFACE('',#7618,0.425);
#6011=CYLINDRICAL_SURFACE('',#7628,0.275);
#6012=CYLINDRICAL_SURFACE('',#7631,0.275);
#6013=CYLINDRICAL_SURFACE('',#7634,0.275);
#6014=CYLINDRICAL_SURFACE('',#7637,0.275);
#6015=CYLINDRICAL_SURFACE('',#7647,0.5);
#6016=CYLINDRICAL_SURFACE('',#7651,0.6);
#6017=CYLINDRICAL_SURFACE('',#7655,0.605);
#6018=CYLINDRICAL_SURFACE('',#7658,1.25);
#6019=ADVANCED_FACE('',(#901),#5892,.F.);
#6020=ADVANCED_FACE('',(#902),#5893,.F.);
#6021=ADVANCED_FACE('',(#903),#5894,.F.);
#6022=ADVANCED_FACE('',(#904),#5895,.F.);
#6023=ADVANCED_FACE('',(#905),#5896,.F.);
#6024=ADVANCED_FACE('',(#906),#5897,.F.);
#6025=ADVANCED_FACE('',(#907),#681,.F.);
#6026=ADVANCED_FACE('',(#908),#682,.F.);
#6027=ADVANCED_FACE('',(#909),#683,.F.);
#6028=ADVANCED_FACE('',(#910),#684,.F.);
#6029=ADVANCED_FACE('',(#911),#685,.T.);
#6030=ADVANCED_FACE('',(#912),#686,.T.);
#6031=ADVANCED_FACE('',(#913),#687,.T.);
#6032=ADVANCED_FACE('',(#914),#688,.T.);
#6033=ADVANCED_FACE('',(#915),#689,.T.);
#6034=ADVANCED_FACE('',(#916,#507,#508,#509,#510,#511,#512,#513),#690,.T.);
#6035=ADVANCED_FACE('',(#917,#514,#515,#516,#517,#518,#519),#691,.F.);
#6036=ADVANCED_FACE('',(#918),#692,.T.);
#6037=ADVANCED_FACE('',(#919),#693,.T.);
#6038=ADVANCED_FACE('',(#920),#694,.T.);
#6039=ADVANCED_FACE('',(#921),#695,.T.);
#6040=ADVANCED_FACE('',(#922),#696,.T.);
#6041=ADVANCED_FACE('',(#923),#697,.F.);
#6042=ADVANCED_FACE('',(#924),#698,.T.);
#6043=ADVANCED_FACE('',(#925),#699,.T.);
#6044=ADVANCED_FACE('',(#926),#700,.T.);
#6045=ADVANCED_FACE('',(#927),#701,.T.);
#6046=ADVANCED_FACE('',(#928),#702,.T.);
#6047=ADVANCED_FACE('',(#929),#703,.F.);
#6048=ADVANCED_FACE('',(#930),#5898,.F.);
#6049=ADVANCED_FACE('',(#931),#5899,.F.);
#6050=ADVANCED_FACE('',(#932),#5900,.F.);
#6051=ADVANCED_FACE('',(#933),#5901,.F.);
#6052=ADVANCED_FACE('',(#934),#5902,.F.);
#6053=ADVANCED_FACE('',(#935),#5903,.F.);
#6054=ADVANCED_FACE('',(#936),#5904,.F.);
#6055=ADVANCED_FACE('',(#937,#520),#704,.T.);
#6056=ADVANCED_FACE('',(#938,#521),#705,.T.);
#6057=ADVANCED_FACE('',(#939),#706,.T.);
#6058=ADVANCED_FACE('',(#940),#707,.T.);
#6059=ADVANCED_FACE('',(#941,#522,#523,#524,#525,#526),#708,.T.);
#6060=ADVANCED_FACE('',(#942),#709,.T.);
#6061=ADVANCED_FACE('',(#943,#527,#528,#529,#530,#531),#710,.T.);
#6062=ADVANCED_FACE('',(#944),#711,.T.);
#6063=ADVANCED_FACE('',(#945),#712,.T.);
#6064=ADVANCED_FACE('',(#946,#532,#533),#713,.F.);
#6065=ADVANCED_FACE('',(#947),#5905,.F.);
#6066=ADVANCED_FACE('',(#948),#5906,.F.);
#6067=ADVANCED_FACE('',(#949),#5907,.F.);
#6068=ADVANCED_FACE('',(#950),#5908,.F.);
#6069=ADVANCED_FACE('',(#951),#5909,.T.);
#6070=ADVANCED_FACE('',(#952,#534),#714,.T.);
#6071=ADVANCED_FACE('',(#953),#5910,.F.);
#6072=ADVANCED_FACE('',(#954),#5911,.T.);
#6073=ADVANCED_FACE('',(#955,#535,#536,#537,#538,#539),#715,.T.);
#6074=ADVANCED_FACE('',(#956,#540,#541,#542,#543,#544),#716,.F.);
#6075=ADVANCED_FACE('',(#957),#5912,.F.);
#6076=ADVANCED_FACE('',(#958),#5913,.F.);
#6077=ADVANCED_FACE('',(#959),#5914,.F.);
#6078=ADVANCED_FACE('',(#960),#5915,.F.);
#6079=ADVANCED_FACE('',(#961),#5916,.T.);
#6080=ADVANCED_FACE('',(#962,#545),#717,.F.);
#6081=ADVANCED_FACE('',(#963),#5917,.F.);
#6082=ADVANCED_FACE('',(#964),#5918,.T.);
#6083=ADVANCED_FACE('',(#965,#546,#547,#548,#549,#550),#718,.T.);
#6084=ADVANCED_FACE('',(#966,#551,#552,#553,#554,#555),#719,.F.);
#6085=ADVANCED_FACE('',(#967),#5919,.F.);
#6086=ADVANCED_FACE('',(#968),#5920,.F.);
#6087=ADVANCED_FACE('',(#969),#5921,.F.);
#6088=ADVANCED_FACE('',(#970),#5922,.F.);
#6089=ADVANCED_FACE('',(#971),#5923,.F.);
#6090=ADVANCED_FACE('',(#972),#5924,.F.);
#6091=ADVANCED_FACE('',(#973),#5925,.F.);
#6092=ADVANCED_FACE('',(#974,#556),#720,.T.);
#6093=ADVANCED_FACE('',(#975,#557),#721,.T.);
#6094=ADVANCED_FACE('',(#976),#722,.T.);
#6095=ADVANCED_FACE('',(#977),#723,.T.);
#6096=ADVANCED_FACE('',(#978,#558,#559,#560,#561,#562),#724,.T.);
#6097=ADVANCED_FACE('',(#979),#725,.T.);
#6098=ADVANCED_FACE('',(#980,#563,#564,#565,#566,#567),#726,.T.);
#6099=ADVANCED_FACE('',(#981),#727,.T.);
#6100=ADVANCED_FACE('',(#982),#728,.T.);
#6101=ADVANCED_FACE('',(#983,#568,#569),#729,.F.);
#6102=ADVANCED_FACE('',(#984),#5926,.F.);
#6103=ADVANCED_FACE('',(#985),#5927,.F.);
#6104=ADVANCED_FACE('',(#986),#5928,.F.);
#6105=ADVANCED_FACE('',(#987),#5929,.F.);
#6106=ADVANCED_FACE('',(#988),#5930,.T.);
#6107=ADVANCED_FACE('',(#989,#570),#730,.T.);
#6108=ADVANCED_FACE('',(#990),#5931,.F.);
#6109=ADVANCED_FACE('',(#991),#5932,.T.);
#6110=ADVANCED_FACE('',(#992,#571,#572,#573,#574,#575),#731,.T.);
#6111=ADVANCED_FACE('',(#993,#576,#577,#578,#579,#580),#732,.F.);
#6112=ADVANCED_FACE('',(#994),#5933,.F.);
#6113=ADVANCED_FACE('',(#995),#5934,.F.);
#6114=ADVANCED_FACE('',(#996),#5935,.F.);
#6115=ADVANCED_FACE('',(#997),#5936,.F.);
#6116=ADVANCED_FACE('',(#998),#5937,.T.);
#6117=ADVANCED_FACE('',(#999,#581),#733,.F.);
#6118=ADVANCED_FACE('',(#1000),#5938,.F.);
#6119=ADVANCED_FACE('',(#1001),#5939,.T.);
#6120=ADVANCED_FACE('',(#1002,#582,#583,#584,#585,#586),#734,.T.);
#6121=ADVANCED_FACE('',(#1003,#587,#588,#589,#590,#591),#735,.F.);
#6122=ADVANCED_FACE('',(#1004),#5940,.F.);
#6123=ADVANCED_FACE('',(#1005),#736,.T.);
#6124=ADVANCED_FACE('',(#1006),#5941,.F.);
#6125=ADVANCED_FACE('',(#1007),#737,.T.);
#6126=ADVANCED_FACE('',(#1008),#5942,.F.);
#6127=ADVANCED_FACE('',(#1009),#738,.T.);
#6128=ADVANCED_FACE('',(#1010),#5943,.F.);
#6129=ADVANCED_FACE('',(#1011),#739,.T.);
#6130=ADVANCED_FACE('',(#1012),#5944,.F.);
#6131=ADVANCED_FACE('',(#1013,#592),#740,.T.);
#6132=ADVANCED_FACE('',(#1014),#5945,.F.);
#6133=ADVANCED_FACE('',(#1015),#5946,.F.);
#6134=ADVANCED_FACE('',(#1016,#593),#741,.T.);
#6135=ADVANCED_FACE('',(#1017),#5947,.F.);
#6136=ADVANCED_FACE('',(#1018),#5948,.F.);
#6137=ADVANCED_FACE('',(#1019,#594),#742,.T.);
#6138=ADVANCED_FACE('',(#1020),#5949,.F.);
#6139=ADVANCED_FACE('',(#1021,#595),#743,.T.);
#6140=ADVANCED_FACE('',(#1022),#744,.T.);
#6141=ADVANCED_FACE('',(#1023),#745,.F.);
#6142=ADVANCED_FACE('',(#1024),#746,.T.);
#6143=ADVANCED_FACE('',(#1025),#747,.T.);
#6144=ADVANCED_FACE('',(#1026,#596),#748,.T.);
#6145=ADVANCED_FACE('',(#1027),#749,.T.);
#6146=ADVANCED_FACE('',(#1028),#750,.F.);
#6147=ADVANCED_FACE('',(#1029),#751,.T.);
#6148=ADVANCED_FACE('',(#1030),#752,.T.);
#6149=ADVANCED_FACE('',(#1031),#753,.T.);
#6150=ADVANCED_FACE('',(#1032),#754,.T.);
#6151=ADVANCED_FACE('',(#1033,#597,#598,#599,#600,#601,#602,#603),#755,
 .T.);
#6152=ADVANCED_FACE('',(#1034,#604),#756,.F.);
#6153=ADVANCED_FACE('',(#1035),#5950,.F.);
#6154=ADVANCED_FACE('',(#1036),#5951,.T.);
#6155=ADVANCED_FACE('',(#1037,#605),#757,.T.);
#6156=ADVANCED_FACE('',(#1038,#606),#758,.F.);
#6157=ADVANCED_FACE('',(#1039),#5952,.F.);
#6158=ADVANCED_FACE('',(#1040),#5953,.F.);
#6159=ADVANCED_FACE('',(#1041),#5954,.F.);
#6160=ADVANCED_FACE('',(#1042),#5955,.F.);
#6161=ADVANCED_FACE('',(#1043),#5956,.T.);
#6162=ADVANCED_FACE('',(#1044,#607),#759,.F.);
#6163=ADVANCED_FACE('',(#1045),#5957,.F.);
#6164=ADVANCED_FACE('',(#1046),#5958,.T.);
#6165=ADVANCED_FACE('',(#1047,#608,#609,#610,#611,#612),#760,.T.);
#6166=ADVANCED_FACE('',(#1048,#613,#614,#615,#616,#617),#761,.F.);
#6167=ADVANCED_FACE('',(#1049),#347,.T.);
#6168=ADVANCED_FACE('',(#1050),#762,.T.);
#6169=ADVANCED_FACE('',(#1051),#763,.F.);
#6170=ADVANCED_FACE('',(#1052),#330,.F.);
#6171=ADVANCED_FACE('',(#1053),#5959,.T.);
#6172=ADVANCED_FACE('',(#1054),#5960,.F.);
#6173=ADVANCED_FACE('',(#1055),#315,.F.);
#6174=ADVANCED_FACE('',(#1056,#618),#764,.T.);
#6175=ADVANCED_FACE('',(#1057),#5961,.T.);
#6176=ADVANCED_FACE('',(#1058,#619),#765,.T.);
#6177=ADVANCED_FACE('',(#1059),#316,.F.);
#6178=ADVANCED_FACE('',(#1060),#331,.F.);
#6179=ADVANCED_FACE('',(#1061),#5962,.F.);
#6180=ADVANCED_FACE('',(#1062,#620),#766,.T.);
#6181=ADVANCED_FACE('',(#1063),#317,.T.);
#6182=ADVANCED_FACE('',(#1064),#5963,.T.);
#6183=ADVANCED_FACE('',(#1065),#318,.T.);
#6184=ADVANCED_FACE('',(#1066,#621),#767,.T.);
#6185=ADVANCED_FACE('',(#1067),#5964,.F.);
#6186=ADVANCED_FACE('',(#1068),#301,.T.);
#6187=ADVANCED_FACE('',(#1069),#302,.T.);
#6188=ADVANCED_FACE('',(#1070),#303,.T.);
#6189=ADVANCED_FACE('',(#1071),#304,.T.);
#6190=ADVANCED_FACE('',(#1072),#305,.T.);
#6191=ADVANCED_FACE('',(#1073),#306,.T.);
#6192=ADVANCED_FACE('',(#1074),#307,.T.);
#6193=ADVANCED_FACE('',(#1075),#308,.F.);
#6194=ADVANCED_FACE('',(#1076),#5965,.T.);
#6195=ADVANCED_FACE('',(#1077),#768,.T.);
#6196=ADVANCED_FACE('',(#1078),#309,.F.);
#6197=ADVANCED_FACE('',(#1079),#769,.T.);
#6198=ADVANCED_FACE('',(#1080),#310,.F.);
#6199=ADVANCED_FACE('',(#1081),#770,.T.);
#6200=ADVANCED_FACE('',(#1082),#311,.F.);
#6201=ADVANCED_FACE('',(#1083),#771,.T.);
#6202=ADVANCED_FACE('',(#1084),#312,.F.);
#6203=ADVANCED_FACE('',(#1085),#772,.T.);
#6204=ADVANCED_FACE('',(#1086),#313,.F.);
#6205=ADVANCED_FACE('',(#1087),#5966,.F.);
#6206=ADVANCED_FACE('',(#1088),#773,.T.);
#6207=ADVANCED_FACE('',(#1089),#314,.F.);
#6208=ADVANCED_FACE('',(#1090,#622),#774,.T.);
#6209=ADVANCED_FACE('',(#1091),#775,.T.);
#6210=ADVANCED_FACE('',(#1092,#623),#776,.T.);
#6211=ADVANCED_FACE('',(#1093),#5967,.T.);
#6212=ADVANCED_FACE('',(#1094,#624),#777,.T.);
#6213=ADVANCED_FACE('',(#1095),#5968,.F.);
#6214=ADVANCED_FACE('',(#1096,#625),#778,.T.);
#6215=ADVANCED_FACE('',(#1097),#5969,.T.);
#6216=ADVANCED_FACE('',(#1098,#626),#779,.T.);
#6217=ADVANCED_FACE('',(#1099),#5970,.F.);
#6218=ADVANCED_FACE('',(#1100),#780,.T.);
#6219=ADVANCED_FACE('',(#1101),#319,.T.);
#6220=ADVANCED_FACE('',(#1102),#5971,.T.);
#6221=ADVANCED_FACE('',(#1103),#320,.T.);
#6222=ADVANCED_FACE('',(#1104,#627),#781,.T.);
#6223=ADVANCED_FACE('',(#1105),#321,.T.);
#6224=ADVANCED_FACE('',(#1106),#5972,.T.);
#6225=ADVANCED_FACE('',(#1107),#322,.T.);
#6226=ADVANCED_FACE('',(#1108),#782,.T.);
#6227=ADVANCED_FACE('',(#1109),#783,.F.);
#6228=ADVANCED_FACE('',(#1110),#784,.F.);
#6229=ADVANCED_FACE('',(#1111),#785,.F.);
#6230=ADVANCED_FACE('',(#1112),#786,.F.);
#6231=ADVANCED_FACE('',(#1113),#787,.F.);
#6232=ADVANCED_FACE('',(#1114),#788,.F.);
#6233=ADVANCED_FACE('',(#1115),#789,.F.);
#6234=ADVANCED_FACE('',(#1116),#790,.F.);
#6235=ADVANCED_FACE('',(#1117),#791,.F.);
#6236=ADVANCED_FACE('',(#1118),#792,.F.);
#6237=ADVANCED_FACE('',(#1119),#793,.F.);
#6238=ADVANCED_FACE('',(#1120),#794,.F.);
#6239=ADVANCED_FACE('',(#1121),#795,.F.);
#6240=ADVANCED_FACE('',(#1122,#628),#796,.T.);
#6241=ADVANCED_FACE('',(#1123),#5973,.T.);
#6242=ADVANCED_FACE('',(#1124,#629),#797,.T.);
#6243=ADVANCED_FACE('',(#1125),#5974,.T.);
#6244=ADVANCED_FACE('',(#1126,#630),#798,.T.);
#6245=ADVANCED_FACE('',(#1127),#5975,.T.);
#6246=ADVANCED_FACE('',(#1128,#631),#799,.T.);
#6247=ADVANCED_FACE('',(#1129),#5976,.T.);
#6248=ADVANCED_FACE('',(#1130,#632),#800,.T.);
#6249=ADVANCED_FACE('',(#1131),#5977,.T.);
#6250=ADVANCED_FACE('',(#1132,#633),#801,.T.);
#6251=ADVANCED_FACE('',(#1133,#634),#5978,.F.);
#6252=ADVANCED_FACE('',(#1134),#802,.F.);
#6253=ADVANCED_FACE('',(#1135),#803,.F.);
#6254=ADVANCED_FACE('',(#1136),#804,.F.);
#6255=ADVANCED_FACE('',(#1137),#805,.F.);
#6256=ADVANCED_FACE('',(#1138,#635),#806,.T.);
#6257=ADVANCED_FACE('',(#1139,#636),#5979,.T.);
#6258=ADVANCED_FACE('',(#1140,#637),#807,.T.);
#6259=ADVANCED_FACE('',(#1141,#638),#5980,.F.);
#6260=ADVANCED_FACE('',(#1142),#808,.F.);
#6261=ADVANCED_FACE('',(#1143),#809,.F.);
#6262=ADVANCED_FACE('',(#1144),#810,.F.);
#6263=ADVANCED_FACE('',(#1145),#811,.F.);
#6264=ADVANCED_FACE('',(#1146),#812,.F.);
#6265=ADVANCED_FACE('',(#1147),#813,.F.);
#6266=ADVANCED_FACE('',(#1148),#814,.F.);
#6267=ADVANCED_FACE('',(#1149),#815,.F.);
#6268=ADVANCED_FACE('',(#1150),#816,.F.);
#6269=ADVANCED_FACE('',(#1151),#817,.T.);
#6270=ADVANCED_FACE('',(#1152),#323,.T.);
#6271=ADVANCED_FACE('',(#1153),#5981,.T.);
#6272=ADVANCED_FACE('',(#1154),#324,.T.);
#6273=ADVANCED_FACE('',(#1155,#639),#818,.T.);
#6274=ADVANCED_FACE('',(#1156),#325,.T.);
#6275=ADVANCED_FACE('',(#1157),#5982,.T.);
#6276=ADVANCED_FACE('',(#1158),#5983,.F.);
#6277=ADVANCED_FACE('',(#1159),#819,.T.);
#6278=ADVANCED_FACE('',(#1160),#5984,.F.);
#6279=ADVANCED_FACE('',(#1161),#820,.F.);
#6280=ADVANCED_FACE('',(#1162),#821,.F.);
#6281=ADVANCED_FACE('',(#1163),#822,.T.);
#6282=ADVANCED_FACE('',(#1164),#823,.F.);
#6283=ADVANCED_FACE('',(#1165),#824,.F.);
#6284=ADVANCED_FACE('',(#1166),#825,.F.);
#6285=ADVANCED_FACE('',(#1167),#826,.F.);
#6286=ADVANCED_FACE('',(#1168),#827,.T.);
#6287=ADVANCED_FACE('',(#1169),#828,.F.);
#6288=ADVANCED_FACE('',(#1170),#829,.F.);
#6289=ADVANCED_FACE('',(#1171),#830,.F.);
#6290=ADVANCED_FACE('',(#1172,#640,#641),#5985,.T.);
#6291=ADVANCED_FACE('',(#1173,#642),#831,.T.);
#6292=ADVANCED_FACE('',(#1174,#643),#832,.F.);
#6293=ADVANCED_FACE('',(#1175),#5986,.F.);
#6294=ADVANCED_FACE('',(#1176),#5987,.T.);
#6295=ADVANCED_FACE('',(#1177,#644),#833,.T.);
#6296=ADVANCED_FACE('',(#1178,#645),#834,.F.);
#6297=ADVANCED_FACE('',(#1179),#5988,.F.);
#6298=ADVANCED_FACE('',(#1180),#5989,.T.);
#6299=ADVANCED_FACE('',(#1181,#646),#835,.T.);
#6300=ADVANCED_FACE('',(#1182,#647),#836,.F.);
#6301=ADVANCED_FACE('',(#1183),#5990,.F.);
#6302=ADVANCED_FACE('',(#1184),#5991,.T.);
#6303=ADVANCED_FACE('',(#1185,#648),#837,.T.);
#6304=ADVANCED_FACE('',(#1186,#649),#838,.F.);
#6305=ADVANCED_FACE('',(#1187),#5992,.F.);
#6306=ADVANCED_FACE('',(#1188),#5993,.T.);
#6307=ADVANCED_FACE('',(#1189,#650),#839,.T.);
#6308=ADVANCED_FACE('',(#1190,#651),#840,.F.);
#6309=ADVANCED_FACE('',(#1191),#841,.F.);
#6310=ADVANCED_FACE('',(#1192),#842,.F.);
#6311=ADVANCED_FACE('',(#1193),#843,.F.);
#6312=ADVANCED_FACE('',(#1194,#652),#844,.T.);
#6313=ADVANCED_FACE('',(#1195),#5994,.F.);
#6314=ADVANCED_FACE('',(#1196),#5995,.T.);
#6315=ADVANCED_FACE('',(#1197),#5996,.T.);
#6316=ADVANCED_FACE('',(#1198,#653),#845,.F.);
#6317=ADVANCED_FACE('',(#1199),#5997,.T.);
#6318=ADVANCED_FACE('',(#1200,#654),#846,.T.);
#6319=ADVANCED_FACE('',(#1201,#655),#847,.F.);
#6320=ADVANCED_FACE('',(#1202),#5998,.F.);
#6321=ADVANCED_FACE('',(#1203),#848,.F.);
#6322=ADVANCED_FACE('',(#1204),#849,.F.);
#6323=ADVANCED_FACE('',(#1205),#850,.F.);
#6324=ADVANCED_FACE('',(#1206,#656),#851,.T.);
#6325=ADVANCED_FACE('',(#1207),#5999,.F.);
#6326=ADVANCED_FACE('',(#1208),#6000,.T.);
#6327=ADVANCED_FACE('',(#1209,#657),#852,.F.);
#6328=ADVANCED_FACE('',(#1210),#853,.T.);
#6329=ADVANCED_FACE('',(#1211),#854,.T.);
#6330=ADVANCED_FACE('',(#1212,#658),#855,.T.);
#6331=ADVANCED_FACE('',(#1213,#659),#6001,.T.);
#6332=ADVANCED_FACE('',(#1214,#660),#856,.F.);
#6333=ADVANCED_FACE('',(#1215),#6002,.F.);
#6334=ADVANCED_FACE('',(#1216),#857,.F.);
#6335=ADVANCED_FACE('',(#1217),#6003,.T.);
#6336=ADVANCED_FACE('',(#1218),#858,.T.);
#6337=ADVANCED_FACE('',(#1219,#661),#859,.F.);
#6338=ADVANCED_FACE('',(#1220),#6004,.F.);
#6339=ADVANCED_FACE('',(#1221),#6005,.T.);
#6340=ADVANCED_FACE('',(#1222,#662),#860,.T.);
#6341=ADVANCED_FACE('',(#1223,#663),#861,.F.);
#6342=ADVANCED_FACE('',(#1224),#6006,.F.);
#6343=ADVANCED_FACE('',(#1225),#6007,.T.);
#6344=ADVANCED_FACE('',(#1226,#664),#862,.T.);
#6345=ADVANCED_FACE('',(#1227,#665),#863,.F.);
#6346=ADVANCED_FACE('',(#1228),#864,.T.);
#6347=ADVANCED_FACE('',(#1229),#865,.T.);
#6348=ADVANCED_FACE('',(#1230),#866,.T.);
#6349=ADVANCED_FACE('',(#1231),#867,.T.);
#6350=ADVANCED_FACE('',(#1232),#868,.T.);
#6351=ADVANCED_FACE('',(#1233),#869,.F.);
#6352=ADVANCED_FACE('',(#1234),#870,.T.);
#6353=ADVANCED_FACE('',(#1235),#871,.T.);
#6354=ADVANCED_FACE('',(#1236),#872,.T.);
#6355=ADVANCED_FACE('',(#1237),#873,.F.);
#6356=ADVANCED_FACE('',(#1238),#874,.T.);
#6357=ADVANCED_FACE('',(#1239),#326,.T.);
#6358=ADVANCED_FACE('',(#1240),#6008,.T.);
#6359=ADVANCED_FACE('',(#1241),#327,.T.);
#6360=ADVANCED_FACE('',(#1242,#666),#875,.T.);
#6361=ADVANCED_FACE('',(#1243),#328,.T.);
#6362=ADVANCED_FACE('',(#1244),#6009,.T.);
#6363=ADVANCED_FACE('',(#1245),#329,.T.);
#6364=ADVANCED_FACE('',(#1246),#876,.T.);
#6365=ADVANCED_FACE('',(#1247),#877,.F.);
#6366=ADVANCED_FACE('',(#1248),#878,.F.);
#6367=ADVANCED_FACE('',(#1249),#879,.F.);
#6368=ADVANCED_FACE('',(#1250),#880,.F.);
#6369=ADVANCED_FACE('',(#1251),#881,.F.);
#6370=ADVANCED_FACE('',(#1252),#882,.F.);
#6371=ADVANCED_FACE('',(#1253),#883,.F.);
#6372=ADVANCED_FACE('',(#1254),#884,.F.);
#6373=ADVANCED_FACE('',(#1255),#6010,.F.);
#6374=ADVANCED_FACE('',(#1256),#885,.T.);
#6375=ADVANCED_FACE('',(#1257),#886,.T.);
#6376=ADVANCED_FACE('',(#1258),#887,.T.);
#6377=ADVANCED_FACE('',(#1259),#888,.T.);
#6378=ADVANCED_FACE('',(#1260,#667),#889,.T.);
#6379=ADVANCED_FACE('',(#1261,#668),#890,.F.);
#6380=ADVANCED_FACE('',(#1262),#6011,.F.);
#6381=ADVANCED_FACE('',(#1263),#6012,.F.);
#6382=ADVANCED_FACE('',(#1264),#6013,.F.);
#6383=ADVANCED_FACE('',(#1265),#6014,.F.);
#6384=ADVANCED_FACE('',(#1266,#669,#670,#671,#672,#673),#891,.F.);
#6385=ADVANCED_FACE('',(#1267),#892,.T.);
#6386=ADVANCED_FACE('',(#1268),#893,.T.);
#6387=ADVANCED_FACE('',(#1269),#894,.T.);
#6388=ADVANCED_FACE('',(#1270),#895,.T.);
#6389=ADVANCED_FACE('',(#1271,#674,#675,#676,#677),#896,.T.);
#6390=ADVANCED_FACE('',(#1272),#6015,.T.);
#6391=ADVANCED_FACE('',(#1273),#897,.F.);
#6392=ADVANCED_FACE('',(#1274),#6016,.T.);
#6393=ADVANCED_FACE('',(#1275,#678),#898,.F.);
#6394=ADVANCED_FACE('',(#1276),#6017,.F.);
#6395=ADVANCED_FACE('',(#1277),#6018,.T.);
#6396=ADVANCED_FACE('',(#1278,#679),#899,.T.);
#6397=ADVANCED_FACE('',(#1279,#680),#900,.F.);
#6398=CLOSED_SHELL('',(#6019,#6020,#6021,#6022,#6023,#6024,#6025,#6026,
#6027,#6028,#6029,#6030,#6031,#6032,#6033,#6034,#6035));
#6399=CLOSED_SHELL('',(#6036,#6037,#6038,#6039,#6040,#6041));
#6400=CLOSED_SHELL('',(#6042,#6043,#6044,#6045,#6046,#6047));
#6401=CLOSED_SHELL('',(#6048,#6049,#6050,#6051,#6052,#6053,#6054,#6055,
#6056,#6057,#6058,#6059,#6060,#6061,#6062,#6063,#6064));
#6402=CLOSED_SHELL('',(#6065,#6066,#6067,#6068,#6069,#6070,#6071,#6072,
#6073,#6074));
#6403=CLOSED_SHELL('',(#6075,#6076,#6077,#6078,#6079,#6080,#6081,#6082,
#6083,#6084));
#6404=CLOSED_SHELL('',(#6085,#6086,#6087,#6088,#6089,#6090,#6091,#6092,
#6093,#6094,#6095,#6096,#6097,#6098,#6099,#6100,#6101));
#6405=CLOSED_SHELL('',(#6102,#6103,#6104,#6105,#6106,#6107,#6108,#6109,
#6110,#6111));
#6406=CLOSED_SHELL('',(#6112,#6113,#6114,#6115,#6116,#6117,#6118,#6119,
#6120,#6121));
#6407=CLOSED_SHELL('',(#6122,#6123,#6124,#6125,#6126,#6127,#6128,#6129,
#6130,#6131,#6132,#6133,#6134,#6135,#6136,#6137,#6138,#6139,#6140,#6141,
#6142,#6143,#6144,#6145,#6146,#6147,#6148,#6149,#6150,#6151,#6152));
#6408=CLOSED_SHELL('',(#6153,#6154,#6155,#6156));
#6409=CLOSED_SHELL('',(#6157,#6158,#6159,#6160,#6161,#6162,#6163,#6164,
#6165,#6166));
#6410=CLOSED_SHELL('',(#6167,#6168,#6169));
#6411=CLOSED_SHELL('',(#6170,#6171,#6172,#6173,#6174,#6175,#6176,#6177));
#6412=CLOSED_SHELL('',(#6178,#6179,#6180,#6181,#6182,#6183,#6184,#6185));
#6413=CLOSED_SHELL('',(#6186));
#6414=CLOSED_SHELL('',(#6187));
#6415=CLOSED_SHELL('',(#6188));
#6416=CLOSED_SHELL('',(#6189));
#6417=CLOSED_SHELL('',(#6190));
#6418=CLOSED_SHELL('',(#6191));
#6419=CLOSED_SHELL('',(#6192));
#6420=CLOSED_SHELL('',(#6193,#6194,#6195,#6196,#6197,#6198,#6199,#6200,
#6201,#6202,#6203,#6204,#6205,#6206,#6207,#6208,#6209));
#6421=CLOSED_SHELL('',(#6210,#6211,#6212,#6213));
#6422=CLOSED_SHELL('',(#6214,#6215,#6216,#6217));
#6423=CLOSED_SHELL('',(#6218,#6219,#6220,#6221,#6222,#6223,#6224,#6225,
#6226));
#6424=CLOSED_SHELL('',(#6227,#6228,#6229,#6230,#6231,#6232,#6233,#6234));
#6425=CLOSED_SHELL('',(#6235,#6236,#6237,#6238,#6239,#6240,#6241,#6242,
#6243,#6244,#6245,#6246,#6247,#6248,#6249,#6250,#6251));
#6426=CLOSED_SHELL('',(#6252,#6253,#6254,#6255,#6256,#6257,#6258,#6259));
#6427=CLOSED_SHELL('',(#6260,#6261,#6262,#6263,#6264,#6265,#6266,#6267));
#6428=CLOSED_SHELL('',(#6268,#6269,#6270,#6271,#6272,#6273,#6274,#6275));
#6429=CLOSED_SHELL('',(#6276,#6277,#6278,#6279,#6280,#6281,#6282,#6283,
#6284,#6285,#6286,#6287,#6288,#6289,#6290,#6291,#6292));
#6430=CLOSED_SHELL('',(#6293,#6294,#6295,#6296));
#6431=CLOSED_SHELL('',(#6297,#6298,#6299,#6300));
#6432=CLOSED_SHELL('',(#6301,#6302,#6303,#6304));
#6433=CLOSED_SHELL('',(#6305,#6306,#6307,#6308));
#6434=CLOSED_SHELL('',(#6309,#6310,#6311,#6312,#6313,#6314,#6315,#6316,
#6317,#6318,#6319));
#6435=CLOSED_SHELL('',(#6320,#6321,#6322,#6323,#6324,#6325,#6326,#6327,
#6328,#6329,#6330,#6331,#6332));
#6436=CLOSED_SHELL('',(#6333,#6334,#6335,#6336,#6337));
#6437=CLOSED_SHELL('',(#6338,#6339,#6340,#6341));
#6438=CLOSED_SHELL('',(#6342,#6343,#6344,#6345));
#6439=CLOSED_SHELL('',(#6346,#6347,#6348,#6349,#6350,#6351,#6352,#6353,
#6354,#6355));
#6440=CLOSED_SHELL('',(#6356,#6357,#6358,#6359,#6360,#6361,#6362,#6363,
#6364));
#6441=CLOSED_SHELL('',(#6365,#6366,#6367,#6368,#6369,#6370,#6371,#6372));
#6442=CLOSED_SHELL('',(#6373,#6374,#6375,#6376,#6377,#6378,#6379));
#6443=CLOSED_SHELL('',(#6380,#6381,#6382,#6383,#6384,#6385,#6386,#6387,
#6388,#6389,#6390,#6391,#6392,#6393));
#6444=CLOSED_SHELL('',(#6394,#6395,#6396,#6397));
#6445=DERIVED_UNIT_ELEMENT(#6519,1.);
#6446=DERIVED_UNIT_ELEMENT(#13279,-3.);
#6447=DERIVED_UNIT_ELEMENT(#6519,1.);
#6448=DERIVED_UNIT_ELEMENT(#13279,-3.);
#6449=DERIVED_UNIT_ELEMENT(#6519,1.);
#6450=DERIVED_UNIT_ELEMENT(#13279,-3.);
#6451=DERIVED_UNIT_ELEMENT(#6519,1.);
#6452=DERIVED_UNIT_ELEMENT(#13279,-3.);
#6453=DERIVED_UNIT_ELEMENT(#6519,1.);
#6454=DERIVED_UNIT_ELEMENT(#13279,-3.);
#6455=DERIVED_UNIT_ELEMENT(#6519,1.);
#6456=DERIVED_UNIT_ELEMENT(#13279,-3.);
#6457=DERIVED_UNIT_ELEMENT(#6519,1.);
#6458=DERIVED_UNIT_ELEMENT(#13279,-3.);
#6459=DERIVED_UNIT_ELEMENT(#6519,1.);
#6460=DERIVED_UNIT_ELEMENT(#13279,-3.);
#6461=DERIVED_UNIT_ELEMENT(#6519,1.);
#6462=DERIVED_UNIT_ELEMENT(#13279,-3.);
#6463=DERIVED_UNIT_ELEMENT(#6519,1.);
#6464=DERIVED_UNIT_ELEMENT(#13279,-3.);
#6465=DERIVED_UNIT_ELEMENT(#6519,1.);
#6466=DERIVED_UNIT_ELEMENT(#13279,-3.);
#6467=DERIVED_UNIT_ELEMENT(#6519,1.);
#6468=DERIVED_UNIT_ELEMENT(#13279,-3.);
#6469=DERIVED_UNIT_ELEMENT(#6519,1.);
#6470=DERIVED_UNIT_ELEMENT(#13279,-3.);
#6471=DERIVED_UNIT_ELEMENT(#6519,1.);
#6472=DERIVED_UNIT_ELEMENT(#13279,-3.);
#6473=DERIVED_UNIT_ELEMENT(#6519,1.);
#6474=DERIVED_UNIT_ELEMENT(#13279,-3.);
#6475=DERIVED_UNIT_ELEMENT(#6519,1.);
#6476=DERIVED_UNIT_ELEMENT(#13279,-3.);
#6477=DERIVED_UNIT_ELEMENT(#6519,1.);
#6478=DERIVED_UNIT_ELEMENT(#13279,-3.);
#6479=DERIVED_UNIT_ELEMENT(#6519,1.);
#6480=DERIVED_UNIT_ELEMENT(#13279,-3.);
#6481=DERIVED_UNIT_ELEMENT(#6519,1.);
#6482=DERIVED_UNIT_ELEMENT(#13279,-3.);
#6483=DERIVED_UNIT_ELEMENT(#6519,1.);
#6484=DERIVED_UNIT_ELEMENT(#13279,-3.);
#6485=DERIVED_UNIT_ELEMENT(#6519,1.);
#6486=DERIVED_UNIT_ELEMENT(#13279,-3.);
#6487=DERIVED_UNIT_ELEMENT(#6519,1.);
#6488=DERIVED_UNIT_ELEMENT(#13279,-3.);
#6489=DERIVED_UNIT_ELEMENT(#6519,1.);
#6490=DERIVED_UNIT_ELEMENT(#13279,-3.);
#6491=DERIVED_UNIT_ELEMENT(#6519,1.);
#6492=DERIVED_UNIT_ELEMENT(#13279,-3.);
#6493=DERIVED_UNIT_ELEMENT(#6519,1.);
#6494=DERIVED_UNIT_ELEMENT(#13279,-3.);
#6495=DERIVED_UNIT_ELEMENT(#6519,1.);
#6496=DERIVED_UNIT_ELEMENT(#13279,-3.);
#6497=DERIVED_UNIT_ELEMENT(#6519,1.);
#6498=DERIVED_UNIT_ELEMENT(#13279,-3.);
#6499=DERIVED_UNIT_ELEMENT(#6519,1.);
#6500=DERIVED_UNIT_ELEMENT(#13279,-3.);
#6501=DERIVED_UNIT_ELEMENT(#6519,1.);
#6502=DERIVED_UNIT_ELEMENT(#13279,-3.);
#6503=DERIVED_UNIT_ELEMENT(#6519,1.);
#6504=DERIVED_UNIT_ELEMENT(#13279,-3.);
#6505=DERIVED_UNIT_ELEMENT(#6519,1.);
#6506=DERIVED_UNIT_ELEMENT(#13279,-3.);
#6507=DERIVED_UNIT_ELEMENT(#6519,1.);
#6508=DERIVED_UNIT_ELEMENT(#13279,-3.);
#6509=DERIVED_UNIT_ELEMENT(#6519,1.);
#6510=DERIVED_UNIT_ELEMENT(#13279,-3.);
#6511=DERIVED_UNIT_ELEMENT(#6519,1.);
#6512=DERIVED_UNIT_ELEMENT(#13279,-3.);
#6513=DERIVED_UNIT_ELEMENT(#6519,1.);
#6514=DERIVED_UNIT_ELEMENT(#13279,-3.);
#6515=DERIVED_UNIT_ELEMENT(#6519,1.);
#6516=DERIVED_UNIT_ELEMENT(#13279,-3.);
#6517=DERIVED_UNIT_ELEMENT(#6519,1.);
#6518=DERIVED_UNIT_ELEMENT(#13279,-3.);
#6519=(
MASS_UNIT()
NAMED_UNIT(*)
SI_UNIT(.KILO.,.GRAM.)
);
#6520=DERIVED_UNIT((#6445,#6446));
#6521=DERIVED_UNIT((#6447,#6448));
#6522=DERIVED_UNIT((#6449,#6450));
#6523=DERIVED_UNIT((#6451,#6452));
#6524=DERIVED_UNIT((#6453,#6454));
#6525=DERIVED_UNIT((#6455,#6456));
#6526=DERIVED_UNIT((#6457,#6458));
#6527=DERIVED_UNIT((#6459,#6460));
#6528=DERIVED_UNIT((#6461,#6462));
#6529=DERIVED_UNIT((#6463,#6464));
#6530=DERIVED_UNIT((#6465,#6466));
#6531=DERIVED_UNIT((#6467,#6468));
#6532=DERIVED_UNIT((#6469,#6470));
#6533=DERIVED_UNIT((#6471,#6472));
#6534=DERIVED_UNIT((#6473,#6474));
#6535=DERIVED_UNIT((#6475,#6476));
#6536=DERIVED_UNIT((#6477,#6478));
#6537=DERIVED_UNIT((#6479,#6480));
#6538=DERIVED_UNIT((#6481,#6482));
#6539=DERIVED_UNIT((#6483,#6484));
#6540=DERIVED_UNIT((#6485,#6486));
#6541=DERIVED_UNIT((#6487,#6488));
#6542=DERIVED_UNIT((#6489,#6490));
#6543=DERIVED_UNIT((#6491,#6492));
#6544=DERIVED_UNIT((#6493,#6494));
#6545=DERIVED_UNIT((#6495,#6496));
#6546=DERIVED_UNIT((#6497,#6498));
#6547=DERIVED_UNIT((#6499,#6500));
#6548=DERIVED_UNIT((#6501,#6502));
#6549=DERIVED_UNIT((#6503,#6504));
#6550=DERIVED_UNIT((#6505,#6506));
#6551=DERIVED_UNIT((#6507,#6508));
#6552=DERIVED_UNIT((#6509,#6510));
#6553=DERIVED_UNIT((#6511,#6512));
#6554=DERIVED_UNIT((#6513,#6514));
#6555=DERIVED_UNIT((#6515,#6516));
#6556=DERIVED_UNIT((#6517,#6518));
#6557=MEASURE_REPRESENTATION_ITEM('density measure',
POSITIVE_RATIO_MEASURE(7850.),#6520);
#6558=MEASURE_REPRESENTATION_ITEM('density measure',
POSITIVE_RATIO_MEASURE(7850.),#6521);
#6559=MEASURE_REPRESENTATION_ITEM('density measure',
POSITIVE_RATIO_MEASURE(7850.),#6522);
#6560=MEASURE_REPRESENTATION_ITEM('density measure',
POSITIVE_RATIO_MEASURE(7850.),#6523);
#6561=MEASURE_REPRESENTATION_ITEM('density measure',
POSITIVE_RATIO_MEASURE(7850.),#6524);
#6562=MEASURE_REPRESENTATION_ITEM('density measure',
POSITIVE_RATIO_MEASURE(7850.),#6525);
#6563=MEASURE_REPRESENTATION_ITEM('density measure',
POSITIVE_RATIO_MEASURE(7850.),#6526);
#6564=MEASURE_REPRESENTATION_ITEM('density measure',
POSITIVE_RATIO_MEASURE(7850.),#6527);
#6565=MEASURE_REPRESENTATION_ITEM('density measure',
POSITIVE_RATIO_MEASURE(7850.),#6528);
#6566=MEASURE_REPRESENTATION_ITEM('density measure',
POSITIVE_RATIO_MEASURE(7850.),#6529);
#6567=MEASURE_REPRESENTATION_ITEM('density measure',
POSITIVE_RATIO_MEASURE(7850.),#6530);
#6568=MEASURE_REPRESENTATION_ITEM('density measure',
POSITIVE_RATIO_MEASURE(7850.),#6531);
#6569=MEASURE_REPRESENTATION_ITEM('density measure',
POSITIVE_RATIO_MEASURE(7850.),#6532);
#6570=MEASURE_REPRESENTATION_ITEM('density measure',
POSITIVE_RATIO_MEASURE(7850.),#6533);
#6571=MEASURE_REPRESENTATION_ITEM('density measure',
POSITIVE_RATIO_MEASURE(7850.),#6534);
#6572=MEASURE_REPRESENTATION_ITEM('density measure',
POSITIVE_RATIO_MEASURE(7850.),#6535);
#6573=MEASURE_REPRESENTATION_ITEM('density measure',
POSITIVE_RATIO_MEASURE(7850.),#6536);
#6574=MEASURE_REPRESENTATION_ITEM('density measure',
POSITIVE_RATIO_MEASURE(7850.),#6537);
#6575=MEASURE_REPRESENTATION_ITEM('density measure',
POSITIVE_RATIO_MEASURE(7850.),#6538);
#6576=MEASURE_REPRESENTATION_ITEM('density measure',
POSITIVE_RATIO_MEASURE(7850.),#6539);
#6577=MEASURE_REPRESENTATION_ITEM('density measure',
POSITIVE_RATIO_MEASURE(7850.),#6540);
#6578=MEASURE_REPRESENTATION_ITEM('density measure',
POSITIVE_RATIO_MEASURE(7850.),#6541);
#6579=MEASURE_REPRESENTATION_ITEM('density measure',
POSITIVE_RATIO_MEASURE(7850.),#6542);
#6580=MEASURE_REPRESENTATION_ITEM('density measure',
POSITIVE_RATIO_MEASURE(7850.),#6543);
#6581=MEASURE_REPRESENTATION_ITEM('density measure',
POSITIVE_RATIO_MEASURE(7850.),#6544);
#6582=MEASURE_REPRESENTATION_ITEM('density measure',
POSITIVE_RATIO_MEASURE(7850.),#6545);
#6583=MEASURE_REPRESENTATION_ITEM('density measure',
POSITIVE_RATIO_MEASURE(7850.),#6546);
#6584=MEASURE_REPRESENTATION_ITEM('density measure',
POSITIVE_RATIO_MEASURE(7850.),#6547);
#6585=MEASURE_REPRESENTATION_ITEM('density measure',
POSITIVE_RATIO_MEASURE(7850.),#6548);
#6586=MEASURE_REPRESENTATION_ITEM('density measure',
POSITIVE_RATIO_MEASURE(7850.),#6549);
#6587=MEASURE_REPRESENTATION_ITEM('density measure',
POSITIVE_RATIO_MEASURE(7850.),#6550);
#6588=MEASURE_REPRESENTATION_ITEM('density measure',
POSITIVE_RATIO_MEASURE(7850.),#6551);
#6589=MEASURE_REPRESENTATION_ITEM('density measure',
POSITIVE_RATIO_MEASURE(7850.),#6552);
#6590=MEASURE_REPRESENTATION_ITEM('density measure',
POSITIVE_RATIO_MEASURE(7850.),#6553);
#6591=MEASURE_REPRESENTATION_ITEM('density measure',
POSITIVE_RATIO_MEASURE(7850.),#6554);
#6592=MEASURE_REPRESENTATION_ITEM('density measure',
POSITIVE_RATIO_MEASURE(7850.),#6555);
#6593=MEASURE_REPRESENTATION_ITEM('density measure',
POSITIVE_RATIO_MEASURE(7850.),#6556);
#6594=PROPERTY_DEFINITION_REPRESENTATION(#6779,#6668);
#6595=PROPERTY_DEFINITION_REPRESENTATION(#6780,#6669);
#6596=PROPERTY_DEFINITION_REPRESENTATION(#6781,#6670);
#6597=PROPERTY_DEFINITION_REPRESENTATION(#6782,#6671);
#6598=PROPERTY_DEFINITION_REPRESENTATION(#6783,#6672);
#6599=PROPERTY_DEFINITION_REPRESENTATION(#6784,#6673);
#6600=PROPERTY_DEFINITION_REPRESENTATION(#6785,#6674);
#6601=PROPERTY_DEFINITION_REPRESENTATION(#6786,#6675);
#6602=PROPERTY_DEFINITION_REPRESENTATION(#6787,#6676);
#6603=PROPERTY_DEFINITION_REPRESENTATION(#6788,#6677);
#6604=PROPERTY_DEFINITION_REPRESENTATION(#6789,#6678);
#6605=PROPERTY_DEFINITION_REPRESENTATION(#6790,#6679);
#6606=PROPERTY_DEFINITION_REPRESENTATION(#6791,#6680);
#6607=PROPERTY_DEFINITION_REPRESENTATION(#6792,#6681);
#6608=PROPERTY_DEFINITION_REPRESENTATION(#6793,#6682);
#6609=PROPERTY_DEFINITION_REPRESENTATION(#6794,#6683);
#6610=PROPERTY_DEFINITION_REPRESENTATION(#6795,#6684);
#6611=PROPERTY_DEFINITION_REPRESENTATION(#6796,#6685);
#6612=PROPERTY_DEFINITION_REPRESENTATION(#6797,#6686);
#6613=PROPERTY_DEFINITION_REPRESENTATION(#6798,#6687);
#6614=PROPERTY_DEFINITION_REPRESENTATION(#6799,#6688);
#6615=PROPERTY_DEFINITION_REPRESENTATION(#6800,#6689);
#6616=PROPERTY_DEFINITION_REPRESENTATION(#6801,#6690);
#6617=PROPERTY_DEFINITION_REPRESENTATION(#6802,#6691);
#6618=PROPERTY_DEFINITION_REPRESENTATION(#6803,#6692);
#6619=PROPERTY_DEFINITION_REPRESENTATION(#6804,#6693);
#6620=PROPERTY_DEFINITION_REPRESENTATION(#6805,#6694);
#6621=PROPERTY_DEFINITION_REPRESENTATION(#6806,#6695);
#6622=PROPERTY_DEFINITION_REPRESENTATION(#6807,#6696);
#6623=PROPERTY_DEFINITION_REPRESENTATION(#6808,#6697);
#6624=PROPERTY_DEFINITION_REPRESENTATION(#6809,#6698);
#6625=PROPERTY_DEFINITION_REPRESENTATION(#6810,#6699);
#6626=PROPERTY_DEFINITION_REPRESENTATION(#6811,#6700);
#6627=PROPERTY_DEFINITION_REPRESENTATION(#6812,#6701);
#6628=PROPERTY_DEFINITION_REPRESENTATION(#6813,#6702);
#6629=PROPERTY_DEFINITION_REPRESENTATION(#6814,#6703);
#6630=PROPERTY_DEFINITION_REPRESENTATION(#6815,#6704);
#6631=PROPERTY_DEFINITION_REPRESENTATION(#6816,#6705);
#6632=PROPERTY_DEFINITION_REPRESENTATION(#6817,#6706);
#6633=PROPERTY_DEFINITION_REPRESENTATION(#6818,#6707);
#6634=PROPERTY_DEFINITION_REPRESENTATION(#6819,#6708);
#6635=PROPERTY_DEFINITION_REPRESENTATION(#6820,#6709);
#6636=PROPERTY_DEFINITION_REPRESENTATION(#6821,#6710);
#6637=PROPERTY_DEFINITION_REPRESENTATION(#6822,#6711);
#6638=PROPERTY_DEFINITION_REPRESENTATION(#6823,#6712);
#6639=PROPERTY_DEFINITION_REPRESENTATION(#6824,#6713);
#6640=PROPERTY_DEFINITION_REPRESENTATION(#6825,#6714);
#6641=PROPERTY_DEFINITION_REPRESENTATION(#6826,#6715);
#6642=PROPERTY_DEFINITION_REPRESENTATION(#6827,#6716);
#6643=PROPERTY_DEFINITION_REPRESENTATION(#6828,#6717);
#6644=PROPERTY_DEFINITION_REPRESENTATION(#6829,#6718);
#6645=PROPERTY_DEFINITION_REPRESENTATION(#6830,#6719);
#6646=PROPERTY_DEFINITION_REPRESENTATION(#6831,#6720);
#6647=PROPERTY_DEFINITION_REPRESENTATION(#6832,#6721);
#6648=PROPERTY_DEFINITION_REPRESENTATION(#6833,#6722);
#6649=PROPERTY_DEFINITION_REPRESENTATION(#6834,#6723);
#6650=PROPERTY_DEFINITION_REPRESENTATION(#6835,#6724);
#6651=PROPERTY_DEFINITION_REPRESENTATION(#6836,#6725);
#6652=PROPERTY_DEFINITION_REPRESENTATION(#6837,#6726);
#6653=PROPERTY_DEFINITION_REPRESENTATION(#6838,#6727);
#6654=PROPERTY_DEFINITION_REPRESENTATION(#6839,#6728);
#6655=PROPERTY_DEFINITION_REPRESENTATION(#6840,#6729);
#6656=PROPERTY_DEFINITION_REPRESENTATION(#6841,#6730);
#6657=PROPERTY_DEFINITION_REPRESENTATION(#6842,#6731);
#6658=PROPERTY_DEFINITION_REPRESENTATION(#6843,#6732);
#6659=PROPERTY_DEFINITION_REPRESENTATION(#6844,#6733);
#6660=PROPERTY_DEFINITION_REPRESENTATION(#6845,#6734);
#6661=PROPERTY_DEFINITION_REPRESENTATION(#6846,#6735);
#6662=PROPERTY_DEFINITION_REPRESENTATION(#6847,#6736);
#6663=PROPERTY_DEFINITION_REPRESENTATION(#6848,#6737);
#6664=PROPERTY_DEFINITION_REPRESENTATION(#6849,#6738);
#6665=PROPERTY_DEFINITION_REPRESENTATION(#6850,#6739);
#6666=PROPERTY_DEFINITION_REPRESENTATION(#6851,#6740);
#6667=PROPERTY_DEFINITION_REPRESENTATION(#6852,#6741);
#6668=REPRESENTATION('material name',(#6742),#13236);
#6669=REPRESENTATION('density',(#6557),#13236);
#6670=REPRESENTATION('material name',(#6743),#13237);
#6671=REPRESENTATION('density',(#6558),#13237);
#6672=REPRESENTATION('material name',(#6744),#13238);
#6673=REPRESENTATION('density',(#6559),#13238);
#6674=REPRESENTATION('material name',(#6745),#13239);
#6675=REPRESENTATION('density',(#6560),#13239);
#6676=REPRESENTATION('material name',(#6746),#13240);
#6677=REPRESENTATION('density',(#6561),#13240);
#6678=REPRESENTATION('material name',(#6747),#13241);
#6679=REPRESENTATION('density',(#6562),#13241);
#6680=REPRESENTATION('material name',(#6748),#13242);
#6681=REPRESENTATION('density',(#6563),#13242);
#6682=REPRESENTATION('material name',(#6749),#13243);
#6683=REPRESENTATION('density',(#6564),#13243);
#6684=REPRESENTATION('material name',(#6750),#13244);
#6685=REPRESENTATION('density',(#6565),#13244);
#6686=REPRESENTATION('material name',(#6751),#13245);
#6687=REPRESENTATION('density',(#6566),#13245);
#6688=REPRESENTATION('material name',(#6752),#13246);
#6689=REPRESENTATION('density',(#6567),#13246);
#6690=REPRESENTATION('material name',(#6753),#13247);
#6691=REPRESENTATION('density',(#6568),#13247);
#6692=REPRESENTATION('material name',(#6754),#13248);
#6693=REPRESENTATION('density',(#6569),#13248);
#6694=REPRESENTATION('material name',(#6755),#13250);
#6695=REPRESENTATION('density',(#6570),#13250);
#6696=REPRESENTATION('material name',(#6756),#13251);
#6697=REPRESENTATION('density',(#6571),#13251);
#6698=REPRESENTATION('material name',(#6757),#13252);
#6699=REPRESENTATION('density',(#6572),#13252);
#6700=REPRESENTATION('material name',(#6758),#13253);
#6701=REPRESENTATION('density',(#6573),#13253);
#6702=REPRESENTATION('material name',(#6759),#13254);
#6703=REPRESENTATION('density',(#6574),#13254);
#6704=REPRESENTATION('material name',(#6760),#13255);
#6705=REPRESENTATION('density',(#6575),#13255);
#6706=REPRESENTATION('material name',(#6761),#13257);
#6707=REPRESENTATION('density',(#6576),#13257);
#6708=REPRESENTATION('material name',(#6762),#13258);
#6709=REPRESENTATION('density',(#6577),#13258);
#6710=REPRESENTATION('material name',(#6763),#13259);
#6711=REPRESENTATION('density',(#6578),#13259);
#6712=REPRESENTATION('material name',(#6764),#13261);
#6713=REPRESENTATION('density',(#6579),#13261);
#6714=REPRESENTATION('material name',(#6765),#13262);
#6715=REPRESENTATION('density',(#6580),#13262);
#6716=REPRESENTATION('material name',(#6766),#13263);
#6717=REPRESENTATION('density',(#6581),#13263);
#6718=REPRESENTATION('material name',(#6767),#13264);
#6719=REPRESENTATION('density',(#6582),#13264);
#6720=REPRESENTATION('material name',(#6768),#13265);
#6721=REPRESENTATION('density',(#6583),#13265);
#6722=REPRESENTATION('material name',(#6769),#13266);
#6723=REPRESENTATION('density',(#6584),#13266);
#6724=REPRESENTATION('material name',(#6770),#13267);
#6725=REPRESENTATION('density',(#6585),#13267);
#6726=REPRESENTATION('material name',(#6771),#13268);
#6727=REPRESENTATION('density',(#6586),#13268);
#6728=REPRESENTATION('material name',(#6772),#13269);
#6729=REPRESENTATION('density',(#6587),#13269);
#6730=REPRESENTATION('material name',(#6773),#13270);
#6731=REPRESENTATION('density',(#6588),#13270);
#6732=REPRESENTATION('material name',(#6774),#13271);
#6733=REPRESENTATION('density',(#6589),#13271);
#6734=REPRESENTATION('material name',(#6775),#13272);
#6735=REPRESENTATION('density',(#6590),#13272);
#6736=REPRESENTATION('material name',(#6776),#13274);
#6737=REPRESENTATION('density',(#6591),#13274);
#6738=REPRESENTATION('material name',(#6777),#13275);
#6739=REPRESENTATION('density',(#6592),#13275);
#6740=REPRESENTATION('material name',(#6778),#13276);
#6741=REPRESENTATION('density',(#6593),#13276);
#6742=DESCRIPTIVE_REPRESENTATION_ITEM('Steel','Steel');
#6743=DESCRIPTIVE_REPRESENTATION_ITEM('Steel','Steel');
#6744=DESCRIPTIVE_REPRESENTATION_ITEM('Steel','Steel');
#6745=DESCRIPTIVE_REPRESENTATION_ITEM('Steel','Steel');
#6746=DESCRIPTIVE_REPRESENTATION_ITEM('Steel','Steel');
#6747=DESCRIPTIVE_REPRESENTATION_ITEM('Steel','Steel');
#6748=DESCRIPTIVE_REPRESENTATION_ITEM('Steel','Steel');
#6749=DESCRIPTIVE_REPRESENTATION_ITEM('Steel','Steel');
#6750=DESCRIPTIVE_REPRESENTATION_ITEM('Steel','Steel');
#6751=DESCRIPTIVE_REPRESENTATION_ITEM('Steel','Steel');
#6752=DESCRIPTIVE_REPRESENTATION_ITEM('Steel','Steel');
#6753=DESCRIPTIVE_REPRESENTATION_ITEM('Steel','Steel');
#6754=DESCRIPTIVE_REPRESENTATION_ITEM('Steel','Steel');
#6755=DESCRIPTIVE_REPRESENTATION_ITEM('Steel','Steel');
#6756=DESCRIPTIVE_REPRESENTATION_ITEM('Steel','Steel');
#6757=DESCRIPTIVE_REPRESENTATION_ITEM('Steel','Steel');
#6758=DESCRIPTIVE_REPRESENTATION_ITEM('Steel','Steel');
#6759=DESCRIPTIVE_REPRESENTATION_ITEM('Steel','Steel');
#6760=DESCRIPTIVE_REPRESENTATION_ITEM('Steel','Steel');
#6761=DESCRIPTIVE_REPRESENTATION_ITEM('Steel','Steel');
#6762=DESCRIPTIVE_REPRESENTATION_ITEM('Steel','Steel');
#6763=DESCRIPTIVE_REPRESENTATION_ITEM('Steel','Steel');
#6764=DESCRIPTIVE_REPRESENTATION_ITEM('Steel','Steel');
#6765=DESCRIPTIVE_REPRESENTATION_ITEM('Steel','Steel');
#6766=DESCRIPTIVE_REPRESENTATION_ITEM('Steel','Steel');
#6767=DESCRIPTIVE_REPRESENTATION_ITEM('Steel','Steel');
#6768=DESCRIPTIVE_REPRESENTATION_ITEM('Steel','Steel');
#6769=DESCRIPTIVE_REPRESENTATION_ITEM('Steel','Steel');
#6770=DESCRIPTIVE_REPRESENTATION_ITEM('Steel','Steel');
#6771=DESCRIPTIVE_REPRESENTATION_ITEM('Steel','Steel');
#6772=DESCRIPTIVE_REPRESENTATION_ITEM('Steel','Steel');
#6773=DESCRIPTIVE_REPRESENTATION_ITEM('Steel','Steel');
#6774=DESCRIPTIVE_REPRESENTATION_ITEM('Steel','Steel');
#6775=DESCRIPTIVE_REPRESENTATION_ITEM('Steel','Steel');
#6776=DESCRIPTIVE_REPRESENTATION_ITEM('Steel','Steel');
#6777=DESCRIPTIVE_REPRESENTATION_ITEM('Steel','Steel');
#6778=DESCRIPTIVE_REPRESENTATION_ITEM('Steel','Steel');
#6779=PROPERTY_DEFINITION('material property','material name',#13485);
#6780=PROPERTY_DEFINITION('material property','density of part',#13485);
#6781=PROPERTY_DEFINITION('material property','material name',#13486);
#6782=PROPERTY_DEFINITION('material property','density of part',#13486);
#6783=PROPERTY_DEFINITION('material property','material name',#13487);
#6784=PROPERTY_DEFINITION('material property','density of part',#13487);
#6785=PROPERTY_DEFINITION('material property','material name',#13488);
#6786=PROPERTY_DEFINITION('material property','density of part',#13488);
#6787=PROPERTY_DEFINITION('material property','material name',#13489);
#6788=PROPERTY_DEFINITION('material property','density of part',#13489);
#6789=PROPERTY_DEFINITION('material property','material name',#13490);
#6790=PROPERTY_DEFINITION('material property','density of part',#13490);
#6791=PROPERTY_DEFINITION('material property','material name',#13491);
#6792=PROPERTY_DEFINITION('material property','density of part',#13491);
#6793=PROPERTY_DEFINITION('material property','material name',#13492);
#6794=PROPERTY_DEFINITION('material property','density of part',#13492);
#6795=PROPERTY_DEFINITION('material property','material name',#13493);
#6796=PROPERTY_DEFINITION('material property','density of part',#13493);
#6797=PROPERTY_DEFINITION('material property','material name',#13494);
#6798=PROPERTY_DEFINITION('material property','density of part',#13494);
#6799=PROPERTY_DEFINITION('material property','material name',#13495);
#6800=PROPERTY_DEFINITION('material property','density of part',#13495);
#6801=PROPERTY_DEFINITION('material property','material name',#13496);
#6802=PROPERTY_DEFINITION('material property','density of part',#13496);
#6803=PROPERTY_DEFINITION('material property','material name',#13497);
#6804=PROPERTY_DEFINITION('material property','density of part',#13497);
#6805=PROPERTY_DEFINITION('material property','material name',#13499);
#6806=PROPERTY_DEFINITION('material property','density of part',#13499);
#6807=PROPERTY_DEFINITION('material property','material name',#13500);
#6808=PROPERTY_DEFINITION('material property','density of part',#13500);
#6809=PROPERTY_DEFINITION('material property','material name',#13501);
#6810=PROPERTY_DEFINITION('material property','density of part',#13501);
#6811=PROPERTY_DEFINITION('material property','material name',#13502);
#6812=PROPERTY_DEFINITION('material property','density of part',#13502);
#6813=PROPERTY_DEFINITION('material property','material name',#13503);
#6814=PROPERTY_DEFINITION('material property','density of part',#13503);
#6815=PROPERTY_DEFINITION('material property','material name',#13504);
#6816=PROPERTY_DEFINITION('material property','density of part',#13504);
#6817=PROPERTY_DEFINITION('material property','material name',#13506);
#6818=PROPERTY_DEFINITION('material property','density of part',#13506);
#6819=PROPERTY_DEFINITION('material property','material name',#13507);
#6820=PROPERTY_DEFINITION('material property','density of part',#13507);
#6821=PROPERTY_DEFINITION('material property','material name',#13508);
#6822=PROPERTY_DEFINITION('material property','density of part',#13508);
#6823=PROPERTY_DEFINITION('material property','material name',#13510);
#6824=PROPERTY_DEFINITION('material property','density of part',#13510);
#6825=PROPERTY_DEFINITION('material property','material name',#13511);
#6826=PROPERTY_DEFINITION('material property','density of part',#13511);
#6827=PROPERTY_DEFINITION('material property','material name',#13512);
#6828=PROPERTY_DEFINITION('material property','density of part',#13512);
#6829=PROPERTY_DEFINITION('material property','material name',#13513);
#6830=PROPERTY_DEFINITION('material property','density of part',#13513);
#6831=PROPERTY_DEFINITION('material property','material name',#13514);
#6832=PROPERTY_DEFINITION('material property','density of part',#13514);
#6833=PROPERTY_DEFINITION('material property','material name',#13515);
#6834=PROPERTY_DEFINITION('material property','density of part',#13515);
#6835=PROPERTY_DEFINITION('material property','material name',#13516);
#6836=PROPERTY_DEFINITION('material property','density of part',#13516);
#6837=PROPERTY_DEFINITION('material property','material name',#13517);
#6838=PROPERTY_DEFINITION('material property','density of part',#13517);
#6839=PROPERTY_DEFINITION('material property','material name',#13518);
#6840=PROPERTY_DEFINITION('material property','density of part',#13518);
#6841=PROPERTY_DEFINITION('material property','material name',#13519);
#6842=PROPERTY_DEFINITION('material property','density of part',#13519);
#6843=PROPERTY_DEFINITION('material property','material name',#13520);
#6844=PROPERTY_DEFINITION('material property','density of part',#13520);
#6845=PROPERTY_DEFINITION('material property','material name',#13521);
#6846=PROPERTY_DEFINITION('material property','density of part',#13521);
#6847=PROPERTY_DEFINITION('material property','material name',#13523);
#6848=PROPERTY_DEFINITION('material property','density of part',#13523);
#6849=PROPERTY_DEFINITION('material property','material name',#13524);
#6850=PROPERTY_DEFINITION('material property','density of part',#13524);
#6851=PROPERTY_DEFINITION('material property','material name',#13525);
#6852=PROPERTY_DEFINITION('material property','density of part',#13525);
#6853=AXIS2_PLACEMENT_3D('',#9740,#7669,#7670);
#6854=AXIS2_PLACEMENT_3D('',#9741,#7671,#7672);
#6855=AXIS2_PLACEMENT_3D('',#9742,#7673,#7674);
#6856=AXIS2_PLACEMENT_3D('',#9743,#7675,#7676);
#6857=AXIS2_PLACEMENT_3D('',#9745,#7677,#7678);
#6858=AXIS2_PLACEMENT_3D('',#9748,#7680,#7681);
#6859=AXIS2_PLACEMENT_3D('',#9749,#7682,#7683);
#6860=AXIS2_PLACEMENT_3D('',#9751,#7684,#7685);
#6861=AXIS2_PLACEMENT_3D('',#9754,#7687,#7688);
#6862=AXIS2_PLACEMENT_3D('',#9755,#7689,#7690);
#6863=AXIS2_PLACEMENT_3D('',#9757,#7691,#7692);
#6864=AXIS2_PLACEMENT_3D('',#9760,#7694,#7695);
#6865=AXIS2_PLACEMENT_3D('',#9761,#7696,#7697);
#6866=AXIS2_PLACEMENT_3D('',#9763,#7698,#7699);
#6867=AXIS2_PLACEMENT_3D('',#9766,#7701,#7702);
#6868=AXIS2_PLACEMENT_3D('',#9767,#7703,#7704);
#6869=AXIS2_PLACEMENT_3D('',#9769,#7705,#7706);
#6870=AXIS2_PLACEMENT_3D('',#9772,#7708,#7709);
#6871=AXIS2_PLACEMENT_3D('',#9773,#7710,#7711);
#6872=AXIS2_PLACEMENT_3D('',#9775,#7712,#7713);
#6873=AXIS2_PLACEMENT_3D('',#9778,#7715,#7716);
#6874=AXIS2_PLACEMENT_3D('',#9779,#7717,#7718);
#6875=AXIS2_PLACEMENT_3D('',#9788,#7723,#7724);
#6876=AXIS2_PLACEMENT_3D('',#9794,#7728,#7729);
#6877=AXIS2_PLACEMENT_3D('',#9800,#7733,#7734);
#6878=AXIS2_PLACEMENT_3D('',#9803,#7737,#7738);
#6879=AXIS2_PLACEMENT_3D('',#9804,#7739,#7740);
#6880=AXIS2_PLACEMENT_3D('',#9813,#7745,#7746);
#6881=AXIS2_PLACEMENT_3D('',#9819,#7750,#7751);
#6882=AXIS2_PLACEMENT_3D('',#9825,#7755,#7756);
#6883=AXIS2_PLACEMENT_3D('',#9828,#7759,#7760);
#6884=AXIS2_PLACEMENT_3D('',#9829,#7761,#7762);
#6885=AXIS2_PLACEMENT_3D('',#9830,#7763,#7764);
#6886=AXIS2_PLACEMENT_3D('',#9831,#7765,#7766);
#6887=AXIS2_PLACEMENT_3D('',#9840,#7771,#7772);
#6888=AXIS2_PLACEMENT_3D('',#9846,#7776,#7777);
#6889=AXIS2_PLACEMENT_3D('',#9852,#7781,#7782);
#6890=AXIS2_PLACEMENT_3D('',#9855,#7785,#7786);
#6891=AXIS2_PLACEMENT_3D('',#9856,#7787,#7788);
#6892=AXIS2_PLACEMENT_3D('',#9857,#7789,#7790);
#6893=AXIS2_PLACEMENT_3D('',#9858,#7791,#7792);
#6894=AXIS2_PLACEMENT_3D('',#9867,#7797,#7798);
#6895=AXIS2_PLACEMENT_3D('',#9873,#7802,#7803);
#6896=AXIS2_PLACEMENT_3D('',#9879,#7807,#7808);
#6897=AXIS2_PLACEMENT_3D('',#9882,#7811,#7812);
#6898=AXIS2_PLACEMENT_3D('',#9883,#7813,#7814);
#6899=AXIS2_PLACEMENT_3D('',#9884,#7815,#7816);
#6900=AXIS2_PLACEMENT_3D('',#9885,#7817,#7818);
#6901=AXIS2_PLACEMENT_3D('',#9887,#7819,#7820);
#6902=AXIS2_PLACEMENT_3D('',#9890,#7822,#7823);
#6903=AXIS2_PLACEMENT_3D('',#9891,#7824,#7825);
#6904=AXIS2_PLACEMENT_3D('',#9893,#7826,#7827);
#6905=AXIS2_PLACEMENT_3D('',#9896,#7829,#7830);
#6906=AXIS2_PLACEMENT_3D('',#9897,#7831,#7832);
#6907=AXIS2_PLACEMENT_3D('',#9899,#7833,#7834);
#6908=AXIS2_PLACEMENT_3D('',#9902,#7836,#7837);
#6909=AXIS2_PLACEMENT_3D('',#9903,#7838,#7839);
#6910=AXIS2_PLACEMENT_3D('',#9905,#7840,#7841);
#6911=AXIS2_PLACEMENT_3D('',#9908,#7843,#7844);
#6912=AXIS2_PLACEMENT_3D('',#9909,#7845,#7846);
#6913=AXIS2_PLACEMENT_3D('',#9911,#7847,#7848);
#6914=AXIS2_PLACEMENT_3D('',#9914,#7850,#7851);
#6915=AXIS2_PLACEMENT_3D('',#9915,#7852,#7853);
#6916=AXIS2_PLACEMENT_3D('',#9917,#7854,#7855);
#6917=AXIS2_PLACEMENT_3D('',#9920,#7857,#7858);
#6918=AXIS2_PLACEMENT_3D('',#9921,#7859,#7860);
#6919=AXIS2_PLACEMENT_3D('',#9923,#7861,#7862);
#6920=AXIS2_PLACEMENT_3D('',#9926,#7864,#7865);
#6921=AXIS2_PLACEMENT_3D('',#9927,#7866,#7867);
#6922=AXIS2_PLACEMENT_3D('',#9936,#7872,#7873);
#6923=AXIS2_PLACEMENT_3D('',#9945,#7878,#7879);
#6924=AXIS2_PLACEMENT_3D('',#9951,#7883,#7884);
#6925=AXIS2_PLACEMENT_3D('',#9957,#7888,#7889);
#6926=AXIS2_PLACEMENT_3D('',#9964,#7894,#7895);
#6927=AXIS2_PLACEMENT_3D('',#9968,#7898,#7899);
#6928=AXIS2_PLACEMENT_3D('',#9973,#7903,#7904);
#6929=AXIS2_PLACEMENT_3D('',#9975,#7906,#7907);
#6930=AXIS2_PLACEMENT_3D('',#9976,#7908,#7909);
#6931=AXIS2_PLACEMENT_3D('',#9977,#7910,#7911);
#6932=AXIS2_PLACEMENT_3D('',#9978,#7912,#7913);
#6933=AXIS2_PLACEMENT_3D('',#9980,#7914,#7915);
#6934=AXIS2_PLACEMENT_3D('',#9983,#7917,#7918);
#6935=AXIS2_PLACEMENT_3D('',#9984,#7919,#7920);
#6936=AXIS2_PLACEMENT_3D('',#9986,#7921,#7922);
#6937=AXIS2_PLACEMENT_3D('',#9989,#7924,#7925);
#6938=AXIS2_PLACEMENT_3D('',#9990,#7926,#7927);
#6939=AXIS2_PLACEMENT_3D('',#9992,#7928,#7929);
#6940=AXIS2_PLACEMENT_3D('',#9995,#7931,#7932);
#6941=AXIS2_PLACEMENT_3D('',#9996,#7933,#7934);
#6942=AXIS2_PLACEMENT_3D('',#9998,#7935,#7936);
#6943=AXIS2_PLACEMENT_3D('',#10001,#7938,#7939);
#6944=AXIS2_PLACEMENT_3D('',#10002,#7940,#7941);
#6945=AXIS2_PLACEMENT_3D('',#10004,#7942,#7943);
#6946=AXIS2_PLACEMENT_3D('',#10007,#7945,#7946);
#6947=AXIS2_PLACEMENT_3D('',#10008,#7947,#7948);
#6948=AXIS2_PLACEMENT_3D('',#10010,#7949,#7950);
#6949=AXIS2_PLACEMENT_3D('',#10011,#7951,#7952);
#6950=AXIS2_PLACEMENT_3D('',#10014,#7954,#7955);
#6951=AXIS2_PLACEMENT_3D('',#10015,#7956,#7957);
#6952=AXIS2_PLACEMENT_3D('',#10017,#7958,#7959);
#6953=AXIS2_PLACEMENT_3D('',#10020,#7961,#7962);
#6954=AXIS2_PLACEMENT_3D('',#10021,#7963,#7964);
#6955=AXIS2_PLACEMENT_3D('',#10022,#7965,#7966);
#6956=AXIS2_PLACEMENT_3D('',#10023,#7967,#7968);
#6957=AXIS2_PLACEMENT_3D('',#10024,#7969,#7970);
#6958=AXIS2_PLACEMENT_3D('',#10026,#7971,#7972);
#6959=AXIS2_PLACEMENT_3D('',#10029,#7974,#7975);
#6960=AXIS2_PLACEMENT_3D('',#10030,#7976,#7977);
#6961=AXIS2_PLACEMENT_3D('',#10032,#7978,#7979);
#6962=AXIS2_PLACEMENT_3D('',#10035,#7981,#7982);
#6963=AXIS2_PLACEMENT_3D('',#10036,#7983,#7984);
#6964=AXIS2_PLACEMENT_3D('',#10038,#7985,#7986);
#6965=AXIS2_PLACEMENT_3D('',#10041,#7988,#7989);
#6966=AXIS2_PLACEMENT_3D('',#10042,#7990,#7991);
#6967=AXIS2_PLACEMENT_3D('',#10044,#7992,#7993);
#6968=AXIS2_PLACEMENT_3D('',#10047,#7995,#7996);
#6969=AXIS2_PLACEMENT_3D('',#10048,#7997,#7998);
#6970=AXIS2_PLACEMENT_3D('',#10050,#7999,#8000);
#6971=AXIS2_PLACEMENT_3D('',#10053,#8002,#8003);
#6972=AXIS2_PLACEMENT_3D('',#10054,#8004,#8005);
#6973=AXIS2_PLACEMENT_3D('',#10056,#8006,#8007);
#6974=AXIS2_PLACEMENT_3D('',#10057,#8008,#8009);
#6975=AXIS2_PLACEMENT_3D('',#10059,#8010,#8011);
#6976=AXIS2_PLACEMENT_3D('',#10061,#8013,#8014);
#6977=AXIS2_PLACEMENT_3D('',#10063,#8015,#8016);
#6978=AXIS2_PLACEMENT_3D('',#10066,#8018,#8019);
#6979=AXIS2_PLACEMENT_3D('',#10067,#8020,#8021);
#6980=AXIS2_PLACEMENT_3D('',#10068,#8022,#8023);
#6981=AXIS2_PLACEMENT_3D('',#10069,#8024,#8025);
#6982=AXIS2_PLACEMENT_3D('',#10070,#8026,#8027);
#6983=AXIS2_PLACEMENT_3D('',#10072,#8028,#8029);
#6984=AXIS2_PLACEMENT_3D('',#10075,#8031,#8032);
#6985=AXIS2_PLACEMENT_3D('',#10076,#8033,#8034);
#6986=AXIS2_PLACEMENT_3D('',#10078,#8035,#8036);
#6987=AXIS2_PLACEMENT_3D('',#10081,#8038,#8039);
#6988=AXIS2_PLACEMENT_3D('',#10082,#8040,#8041);
#6989=AXIS2_PLACEMENT_3D('',#10084,#8042,#8043);
#6990=AXIS2_PLACEMENT_3D('',#10087,#8045,#8046);
#6991=AXIS2_PLACEMENT_3D('',#10088,#8047,#8048);
#6992=AXIS2_PLACEMENT_3D('',#10090,#8049,#8050);
#6993=AXIS2_PLACEMENT_3D('',#10093,#8052,#8053);
#6994=AXIS2_PLACEMENT_3D('',#10094,#8054,#8055);
#6995=AXIS2_PLACEMENT_3D('',#10096,#8056,#8057);
#6996=AXIS2_PLACEMENT_3D('',#10099,#8059,#8060);
#6997=AXIS2_PLACEMENT_3D('',#10100,#8061,#8062);
#6998=AXIS2_PLACEMENT_3D('',#10102,#8063,#8064);
#6999=AXIS2_PLACEMENT_3D('',#10105,#8066,#8067);
#7000=AXIS2_PLACEMENT_3D('',#10106,#8068,#8069);
#7001=AXIS2_PLACEMENT_3D('',#10108,#8070,#8071);
#7002=AXIS2_PLACEMENT_3D('',#10111,#8073,#8074);
#7003=AXIS2_PLACEMENT_3D('',#10112,#8075,#8076);
#7004=AXIS2_PLACEMENT_3D('',#10121,#8081,#8082);
#7005=AXIS2_PLACEMENT_3D('',#10130,#8087,#8088);
#7006=AXIS2_PLACEMENT_3D('',#10136,#8092,#8093);
#7007=AXIS2_PLACEMENT_3D('',#10142,#8097,#8098);
#7008=AXIS2_PLACEMENT_3D('',#10149,#8103,#8104);
#7009=AXIS2_PLACEMENT_3D('',#10153,#8107,#8108);
#7010=AXIS2_PLACEMENT_3D('',#10158,#8112,#8113);
#7011=AXIS2_PLACEMENT_3D('',#10160,#8115,#8116);
#7012=AXIS2_PLACEMENT_3D('',#10161,#8117,#8118);
#7013=AXIS2_PLACEMENT_3D('',#10162,#8119,#8120);
#7014=AXIS2_PLACEMENT_3D('',#10163,#8121,#8122);
#7015=AXIS2_PLACEMENT_3D('',#10165,#8123,#8124);
#7016=AXIS2_PLACEMENT_3D('',#10168,#8126,#8127);
#7017=AXIS2_PLACEMENT_3D('',#10169,#8128,#8129);
#7018=AXIS2_PLACEMENT_3D('',#10171,#8130,#8131);
#7019=AXIS2_PLACEMENT_3D('',#10174,#8133,#8134);
#7020=AXIS2_PLACEMENT_3D('',#10175,#8135,#8136);
#7021=AXIS2_PLACEMENT_3D('',#10177,#8137,#8138);
#7022=AXIS2_PLACEMENT_3D('',#10180,#8140,#8141);
#7023=AXIS2_PLACEMENT_3D('',#10181,#8142,#8143);
#7024=AXIS2_PLACEMENT_3D('',#10183,#8144,#8145);
#7025=AXIS2_PLACEMENT_3D('',#10186,#8147,#8148);
#7026=AXIS2_PLACEMENT_3D('',#10187,#8149,#8150);
#7027=AXIS2_PLACEMENT_3D('',#10189,#8151,#8152);
#7028=AXIS2_PLACEMENT_3D('',#10192,#8154,#8155);
#7029=AXIS2_PLACEMENT_3D('',#10193,#8156,#8157);
#7030=AXIS2_PLACEMENT_3D('',#10195,#8158,#8159);
#7031=AXIS2_PLACEMENT_3D('',#10196,#8160,#8161);
#7032=AXIS2_PLACEMENT_3D('',#10199,#8163,#8164);
#7033=AXIS2_PLACEMENT_3D('',#10200,#8165,#8166);
#7034=AXIS2_PLACEMENT_3D('',#10202,#8167,#8168);
#7035=AXIS2_PLACEMENT_3D('',#10205,#8170,#8171);
#7036=AXIS2_PLACEMENT_3D('',#10206,#8172,#8173);
#7037=AXIS2_PLACEMENT_3D('',#10207,#8174,#8175);
#7038=AXIS2_PLACEMENT_3D('',#10208,#8176,#8177);
#7039=AXIS2_PLACEMENT_3D('',#10209,#8178,#8179);
#7040=AXIS2_PLACEMENT_3D('',#10211,#8180,#8181);
#7041=AXIS2_PLACEMENT_3D('',#10214,#8183,#8184);
#7042=AXIS2_PLACEMENT_3D('',#10215,#8185,#8186);
#7043=AXIS2_PLACEMENT_3D('',#10217,#8187,#8188);
#7044=AXIS2_PLACEMENT_3D('',#10220,#8190,#8191);
#7045=AXIS2_PLACEMENT_3D('',#10221,#8192,#8193);
#7046=AXIS2_PLACEMENT_3D('',#10223,#8194,#8195);
#7047=AXIS2_PLACEMENT_3D('',#10226,#8197,#8198);
#7048=AXIS2_PLACEMENT_3D('',#10227,#8199,#8200);
#7049=AXIS2_PLACEMENT_3D('',#10229,#8201,#8202);
#7050=AXIS2_PLACEMENT_3D('',#10232,#8204,#8205);
#7051=AXIS2_PLACEMENT_3D('',#10233,#8206,#8207);
#7052=AXIS2_PLACEMENT_3D('',#10235,#8208,#8209);
#7053=AXIS2_PLACEMENT_3D('',#10238,#8211,#8212);
#7054=AXIS2_PLACEMENT_3D('',#10239,#8213,#8214);
#7055=AXIS2_PLACEMENT_3D('',#10241,#8215,#8216);
#7056=AXIS2_PLACEMENT_3D('',#10242,#8217,#8218);
#7057=AXIS2_PLACEMENT_3D('',#10244,#8219,#8220);
#7058=AXIS2_PLACEMENT_3D('',#10246,#8222,#8223);
#7059=AXIS2_PLACEMENT_3D('',#10248,#8224,#8225);
#7060=AXIS2_PLACEMENT_3D('',#10251,#8227,#8228);
#7061=AXIS2_PLACEMENT_3D('',#10252,#8229,#8230);
#7062=AXIS2_PLACEMENT_3D('',#10253,#8231,#8232);
#7063=AXIS2_PLACEMENT_3D('',#10254,#8233,#8234);
#7064=AXIS2_PLACEMENT_3D('',#10255,#8235,#8236);
#7065=AXIS2_PLACEMENT_3D('',#10257,#8237,#8238);
#7066=AXIS2_PLACEMENT_3D('',#10260,#8240,#8241);
#7067=AXIS2_PLACEMENT_3D('',#10261,#8242,#8243);
#7068=AXIS2_PLACEMENT_3D('',#10262,#8244,#8245);
#7069=AXIS2_PLACEMENT_3D('',#10264,#8246,#8247);
#7070=AXIS2_PLACEMENT_3D('',#10267,#8249,#8250);
#7071=AXIS2_PLACEMENT_3D('',#10268,#8251,#8252);
#7072=AXIS2_PLACEMENT_3D('',#10269,#8253,#8254);
#7073=AXIS2_PLACEMENT_3D('',#10271,#8255,#8256);
#7074=AXIS2_PLACEMENT_3D('',#10274,#8258,#8259);
#7075=AXIS2_PLACEMENT_3D('',#10275,#8260,#8261);
#7076=AXIS2_PLACEMENT_3D('',#10276,#8262,#8263);
#7077=AXIS2_PLACEMENT_3D('',#10278,#8264,#8265);
#7078=AXIS2_PLACEMENT_3D('',#10281,#8267,#8268);
#7079=AXIS2_PLACEMENT_3D('',#10282,#8269,#8270);
#7080=AXIS2_PLACEMENT_3D('',#10283,#8271,#8272);
#7081=AXIS2_PLACEMENT_3D('',#10285,#8273,#8274);
#7082=AXIS2_PLACEMENT_3D('',#10288,#8276,#8277);
#7083=AXIS2_PLACEMENT_3D('',#10289,#8278,#8279);
#7084=AXIS2_PLACEMENT_3D('',#10291,#8280,#8281);
#7085=AXIS2_PLACEMENT_3D('',#10292,#8282,#8283);
#7086=AXIS2_PLACEMENT_3D('',#10294,#8284,#8285);
#7087=AXIS2_PLACEMENT_3D('',#10296,#8287,#8288);
#7088=AXIS2_PLACEMENT_3D('',#10298,#8289,#8290);
#7089=AXIS2_PLACEMENT_3D('',#10301,#8292,#8293);
#7090=AXIS2_PLACEMENT_3D('',#10302,#8294,#8295);
#7091=AXIS2_PLACEMENT_3D('',#10304,#8296,#8297);
#7092=AXIS2_PLACEMENT_3D('',#10305,#8298,#8299);
#7093=AXIS2_PLACEMENT_3D('',#10307,#8300,#8301);
#7094=AXIS2_PLACEMENT_3D('',#10309,#8303,#8304);
#7095=AXIS2_PLACEMENT_3D('',#10311,#8305,#8306);
#7096=AXIS2_PLACEMENT_3D('',#10314,#8308,#8309);
#7097=AXIS2_PLACEMENT_3D('',#10315,#8310,#8311);
#7098=AXIS2_PLACEMENT_3D('',#10317,#8312,#8313);
#7099=AXIS2_PLACEMENT_3D('',#10318,#8314,#8315);
#7100=AXIS2_PLACEMENT_3D('',#10320,#8316,#8317);
#7101=AXIS2_PLACEMENT_3D('',#10322,#8319,#8320);
#7102=AXIS2_PLACEMENT_3D('',#10347,#8333,#8334);
#7103=AXIS2_PLACEMENT_3D('',#10353,#8338,#8339);
#7104=AXIS2_PLACEMENT_3D('',#10359,#8343,#8344);
#7105=AXIS2_PLACEMENT_3D('',#10365,#8348,#8349);
#7106=AXIS2_PLACEMENT_3D('',#10369,#8352,#8353);
#7107=AXIS2_PLACEMENT_3D('',#10373,#8356,#8357);
#7108=AXIS2_PLACEMENT_3D('',#10376,#8360,#8361);
#7109=AXIS2_PLACEMENT_3D('',#10377,#8362,#8363);
#7110=AXIS2_PLACEMENT_3D('',#10383,#8367,#8368);
#7111=AXIS2_PLACEMENT_3D('',#10387,#8371,#8372);
#7112=AXIS2_PLACEMENT_3D('',#10391,#8375,#8376);
#7113=AXIS2_PLACEMENT_3D('',#10394,#8379,#8380);
#7114=AXIS2_PLACEMENT_3D('',#10395,#8381,#8382);
#7115=AXIS2_PLACEMENT_3D('',#10396,#8383,#8384);
#7116=AXIS2_PLACEMENT_3D('',#10397,#8385,#8386);
#7117=AXIS2_PLACEMENT_3D('',#10399,#8387,#8388);
#7118=AXIS2_PLACEMENT_3D('',#10402,#8390,#8391);
#7119=AXIS2_PLACEMENT_3D('',#10403,#8392,#8393);
#7120=AXIS2_PLACEMENT_3D('',#10405,#8394,#8395);
#7121=AXIS2_PLACEMENT_3D('',#10408,#8397,#8398);
#7122=AXIS2_PLACEMENT_3D('',#10409,#8399,#8400);
#7123=AXIS2_PLACEMENT_3D('',#10410,#8401,#8402);
#7124=AXIS2_PLACEMENT_3D('',#10411,#8403,#8404);
#7125=AXIS2_PLACEMENT_3D('',#10412,#8405,#8406);
#7126=AXIS2_PLACEMENT_3D('',#10414,#8407,#8408);
#7127=AXIS2_PLACEMENT_3D('',#10417,#8410,#8411);
#7128=AXIS2_PLACEMENT_3D('',#10418,#8412,#8413);
#7129=AXIS2_PLACEMENT_3D('',#10420,#8414,#8415);
#7130=AXIS2_PLACEMENT_3D('',#10423,#8417,#8418);
#7131=AXIS2_PLACEMENT_3D('',#10424,#8419,#8420);
#7132=AXIS2_PLACEMENT_3D('',#10426,#8421,#8422);
#7133=AXIS2_PLACEMENT_3D('',#10429,#8424,#8425);
#7134=AXIS2_PLACEMENT_3D('',#10430,#8426,#8427);
#7135=AXIS2_PLACEMENT_3D('',#10432,#8428,#8429);
#7136=AXIS2_PLACEMENT_3D('',#10435,#8431,#8432);
#7137=AXIS2_PLACEMENT_3D('',#10436,#8433,#8434);
#7138=AXIS2_PLACEMENT_3D('',#10438,#8435,#8436);
#7139=AXIS2_PLACEMENT_3D('',#10441,#8438,#8439);
#7140=AXIS2_PLACEMENT_3D('',#10442,#8440,#8441);
#7141=AXIS2_PLACEMENT_3D('',#10444,#8442,#8443);
#7142=AXIS2_PLACEMENT_3D('',#10445,#8444,#8445);
#7143=AXIS2_PLACEMENT_3D('',#10447,#8446,#8447);
#7144=AXIS2_PLACEMENT_3D('',#10449,#8449,#8450);
#7145=AXIS2_PLACEMENT_3D('',#10451,#8451,#8452);
#7146=AXIS2_PLACEMENT_3D('',#10454,#8454,#8455);
#7147=AXIS2_PLACEMENT_3D('',#10455,#8456,#8457);
#7148=AXIS2_PLACEMENT_3D('',#10456,#8458,#8459);
#7149=AXIS2_PLACEMENT_3D('',#10457,#8460,#8461);
#7150=AXIS2_PLACEMENT_3D('',#11699,#8462,#8463);
#7151=AXIS2_PLACEMENT_3D('',#11825,#8464,#8465);
#7152=AXIS2_PLACEMENT_3D('',#11826,#8466,#8467);
#7153=AXIS2_PLACEMENT_3D('',#11827,#8468,#8469);
#7154=AXIS2_PLACEMENT_3D('',#11828,#8470,#8471);
#7155=AXIS2_PLACEMENT_3D('',#11829,#8472,#8473);
#7156=AXIS2_PLACEMENT_3D('',#11830,#8474,#8475);
#7157=AXIS2_PLACEMENT_3D('',#11833,#8476,#8477);
#7158=AXIS2_PLACEMENT_3D('',#11834,#8478,#8479);
#7159=AXIS2_PLACEMENT_3D('',#11836,#8480,#8481);
#7160=AXIS2_PLACEMENT_3D('',#11838,#8482,#8483);
#7161=AXIS2_PLACEMENT_3D('',#11839,#8484,#8485);
#7162=AXIS2_PLACEMENT_3D('',#11840,#8486,#8487);
#7163=AXIS2_PLACEMENT_3D('',#11843,#8489,#8490);
#7164=AXIS2_PLACEMENT_3D('',#11844,#8491,#8492);
#7165=AXIS2_PLACEMENT_3D('',#11846,#8493,#8494);
#7166=AXIS2_PLACEMENT_3D('',#11849,#8496,#8497);
#7167=AXIS2_PLACEMENT_3D('',#11850,#8498,#8499);
#7168=AXIS2_PLACEMENT_3D('',#11853,#8501,#8502);
#7169=AXIS2_PLACEMENT_3D('',#11854,#8503,#8504);
#7170=AXIS2_PLACEMENT_3D('',#11855,#8505,#8506);
#7171=AXIS2_PLACEMENT_3D('',#11857,#8507,#8508);
#7172=AXIS2_PLACEMENT_3D('',#11859,#8510,#8511);
#7173=AXIS2_PLACEMENT_3D('',#11861,#8512,#8513);
#7174=AXIS2_PLACEMENT_3D('',#11862,#8514,#8515);
#7175=AXIS2_PLACEMENT_3D('',#11864,#8517,#8518);
#7176=AXIS2_PLACEMENT_3D('',#11865,#8519,#8520);
#7177=AXIS2_PLACEMENT_3D('',#11868,#8521,#8522);
#7178=AXIS2_PLACEMENT_3D('',#11869,#8523,#8524);
#7179=AXIS2_PLACEMENT_3D('',#11871,#8525,#8526);
#7180=AXIS2_PLACEMENT_3D('',#11873,#8527,#8528);
#7181=AXIS2_PLACEMENT_3D('',#11874,#8529,#8530);
#7182=AXIS2_PLACEMENT_3D('',#11875,#8531,#8532);
#7183=AXIS2_PLACEMENT_3D('',#11877,#8533,#8534);
#7184=AXIS2_PLACEMENT_3D('',#11879,#8536,#8537);
#7185=AXIS2_PLACEMENT_3D('',#11881,#8538,#8539);
#7186=AXIS2_PLACEMENT_3D('',#11883,#8540,#8541);
#7187=AXIS2_PLACEMENT_3D('',#11884,#8542,#8543);
#7188=AXIS2_PLACEMENT_3D('',#11886,#8544,#8545);
#7189=AXIS2_PLACEMENT_3D('',#11888,#8547,#8548);
#7190=AXIS2_PLACEMENT_3D('',#11890,#8549,#8550);
#7191=AXIS2_PLACEMENT_3D('',#11892,#8552,#8553);
#7192=AXIS2_PLACEMENT_3D('',#11894,#8554,#8555);
#7193=AXIS2_PLACEMENT_3D('',#11896,#8557,#8558);
#7194=AXIS2_PLACEMENT_3D('',#11897,#8559,#8560);
#7195=AXIS2_PLACEMENT_3D('',#11899,#8562,#8563);
#7196=AXIS2_PLACEMENT_3D('',#11900,#8564,#8565);
#7197=AXIS2_PLACEMENT_3D('',#11903,#8566,#8567);
#7198=AXIS2_PLACEMENT_3D('',#11904,#8568,#8569);
#7199=AXIS2_PLACEMENT_3D('',#11907,#8570,#8571);
#7200=AXIS2_PLACEMENT_3D('',#11908,#8572,#8573);
#7201=AXIS2_PLACEMENT_3D('',#11911,#8574,#8575);
#7202=AXIS2_PLACEMENT_3D('',#11912,#8576,#8577);
#7203=AXIS2_PLACEMENT_3D('',#11915,#8578,#8579);
#7204=AXIS2_PLACEMENT_3D('',#11916,#8580,#8581);
#7205=AXIS2_PLACEMENT_3D('',#11919,#8582,#8583);
#7206=AXIS2_PLACEMENT_3D('',#11920,#8584,#8585);
#7207=AXIS2_PLACEMENT_3D('',#11923,#8586,#8587);
#7208=AXIS2_PLACEMENT_3D('',#11924,#8588,#8589);
#7209=AXIS2_PLACEMENT_3D('',#11927,#8590,#8591);
#7210=AXIS2_PLACEMENT_3D('',#11928,#8592,#8593);
#7211=AXIS2_PLACEMENT_3D('',#11929,#8594,#8595);
#7212=AXIS2_PLACEMENT_3D('',#11955,#8596,#8597);
#7213=AXIS2_PLACEMENT_3D('',#11979,#8598,#8599);
#7214=AXIS2_PLACEMENT_3D('',#11980,#8600,#8601);
#7215=AXIS2_PLACEMENT_3D('',#11982,#8602,#8603);
#7216=AXIS2_PLACEMENT_3D('',#12007,#8604,#8605);
#7217=AXIS2_PLACEMENT_3D('',#12032,#8606,#8607);
#7218=AXIS2_PLACEMENT_3D('',#12035,#8609,#8610);
#7219=AXIS2_PLACEMENT_3D('',#12037,#8611,#8612);
#7220=AXIS2_PLACEMENT_3D('',#12062,#8613,#8614);
#7221=AXIS2_PLACEMENT_3D('',#12087,#8615,#8616);
#7222=AXIS2_PLACEMENT_3D('',#12112,#8617,#8618);
#7223=AXIS2_PLACEMENT_3D('',#12136,#8619,#8620);
#7224=AXIS2_PLACEMENT_3D('',#12137,#8621,#8622);
#7225=AXIS2_PLACEMENT_3D('',#12139,#8623,#8624);
#7226=AXIS2_PLACEMENT_3D('',#12140,#8625,#8626);
#7227=AXIS2_PLACEMENT_3D('',#12141,#8627,#8628);
#7228=AXIS2_PLACEMENT_3D('',#12165,#8629,#8630);
#7229=AXIS2_PLACEMENT_3D('',#12166,#8631,#8632);
#7230=AXIS2_PLACEMENT_3D('',#12168,#8633,#8634);
#7231=AXIS2_PLACEMENT_3D('',#12169,#8635,#8636);
#7232=AXIS2_PLACEMENT_3D('',#12170,#8637,#8638);
#7233=AXIS2_PLACEMENT_3D('',#12194,#8639,#8640);
#7234=AXIS2_PLACEMENT_3D('',#12195,#8641,#8642);
#7235=AXIS2_PLACEMENT_3D('',#12197,#8643,#8644);
#7236=AXIS2_PLACEMENT_3D('',#12199,#8645,#8646);
#7237=AXIS2_PLACEMENT_3D('',#12200,#8647,#8648);
#7238=AXIS2_PLACEMENT_3D('',#12201,#8649,#8650);
#7239=AXIS2_PLACEMENT_3D('',#12225,#8651,#8652);
#7240=AXIS2_PLACEMENT_3D('',#12226,#8653,#8654);
#7241=AXIS2_PLACEMENT_3D('',#12228,#8655,#8656);
#7242=AXIS2_PLACEMENT_3D('',#12229,#8657,#8658);
#7243=AXIS2_PLACEMENT_3D('',#12230,#8659,#8660);
#7244=AXIS2_PLACEMENT_3D('',#12254,#8661,#8662);
#7245=AXIS2_PLACEMENT_3D('',#12255,#8663,#8664);
#7246=AXIS2_PLACEMENT_3D('',#12257,#8665,#8666);
#7247=AXIS2_PLACEMENT_3D('',#12258,#8667,#8668);
#7248=AXIS2_PLACEMENT_3D('',#12259,#8669,#8670);
#7249=AXIS2_PLACEMENT_3D('',#12283,#8671,#8672);
#7250=AXIS2_PLACEMENT_3D('',#12284,#8673,#8674);
#7251=AXIS2_PLACEMENT_3D('',#12286,#8675,#8676);
#7252=AXIS2_PLACEMENT_3D('',#12289,#8678,#8679);
#7253=AXIS2_PLACEMENT_3D('',#12313,#8680,#8681);
#7254=AXIS2_PLACEMENT_3D('',#12314,#8682,#8683);
#7255=AXIS2_PLACEMENT_3D('',#12315,#8684,#8685);
#7256=AXIS2_PLACEMENT_3D('',#12316,#8686,#8687);
#7257=AXIS2_PLACEMENT_3D('',#12317,#8688,#8689);
#7258=AXIS2_PLACEMENT_3D('',#12318,#8690,#8691);
#7259=AXIS2_PLACEMENT_3D('',#12319,#8692,#8693);
#7260=AXIS2_PLACEMENT_3D('',#12320,#8694,#8695);
#7261=AXIS2_PLACEMENT_3D('',#12321,#8696,#8697);
#7262=AXIS2_PLACEMENT_3D('',#12323,#8698,#8699);
#7263=AXIS2_PLACEMENT_3D('',#12325,#8700,#8701);
#7264=AXIS2_PLACEMENT_3D('',#12326,#8702,#8703);
#7265=AXIS2_PLACEMENT_3D('',#12328,#8704,#8705);
#7266=AXIS2_PLACEMENT_3D('',#12330,#8707,#8708);
#7267=AXIS2_PLACEMENT_3D('',#12332,#8709,#8710);
#7268=AXIS2_PLACEMENT_3D('',#12333,#8711,#8712);
#7269=AXIS2_PLACEMENT_3D('',#12335,#8714,#8715);
#7270=AXIS2_PLACEMENT_3D('',#12337,#8716,#8717);
#7271=AXIS2_PLACEMENT_3D('',#12339,#8718,#8719);
#7272=AXIS2_PLACEMENT_3D('',#12340,#8720,#8721);
#7273=AXIS2_PLACEMENT_3D('',#12342,#8722,#8723);
#7274=AXIS2_PLACEMENT_3D('',#12344,#8725,#8726);
#7275=AXIS2_PLACEMENT_3D('',#12346,#8727,#8728);
#7276=AXIS2_PLACEMENT_3D('',#12347,#8729,#8730);
#7277=AXIS2_PLACEMENT_3D('',#12349,#8732,#8733);
#7278=AXIS2_PLACEMENT_3D('',#12350,#8734,#8735);
#7279=AXIS2_PLACEMENT_3D('',#12351,#8736,#8737);
#7280=AXIS2_PLACEMENT_3D('',#12352,#8738,#8739);
#7281=AXIS2_PLACEMENT_3D('',#12353,#8740,#8741);
#7282=AXIS2_PLACEMENT_3D('',#12354,#8742,#8743);
#7283=AXIS2_PLACEMENT_3D('',#12355,#8744,#8745);
#7284=AXIS2_PLACEMENT_3D('',#12357,#8746,#8747);
#7285=AXIS2_PLACEMENT_3D('',#12358,#8748,#8749);
#7286=AXIS2_PLACEMENT_3D('',#12360,#8750,#8751);
#7287=AXIS2_PLACEMENT_3D('',#12362,#8753,#8754);
#7288=AXIS2_PLACEMENT_3D('',#12364,#8755,#8756);
#7289=AXIS2_PLACEMENT_3D('',#12366,#8758,#8759);
#7290=AXIS2_PLACEMENT_3D('',#12368,#8760,#8761);
#7291=AXIS2_PLACEMENT_3D('',#12370,#8763,#8764);
#7292=AXIS2_PLACEMENT_3D('',#12372,#8765,#8766);
#7293=AXIS2_PLACEMENT_3D('',#12373,#8767,#8768);
#7294=AXIS2_PLACEMENT_3D('',#12375,#8769,#8770);
#7295=AXIS2_PLACEMENT_3D('',#12377,#8772,#8773);
#7296=AXIS2_PLACEMENT_3D('',#12379,#8774,#8775);
#7297=AXIS2_PLACEMENT_3D('',#12381,#8777,#8778);
#7298=AXIS2_PLACEMENT_3D('',#12383,#8779,#8780);
#7299=AXIS2_PLACEMENT_3D('',#12385,#8782,#8783);
#7300=AXIS2_PLACEMENT_3D('',#12386,#8784,#8785);
#7301=AXIS2_PLACEMENT_3D('',#12395,#8790,#8791);
#7302=AXIS2_PLACEMENT_3D('',#12401,#8795,#8796);
#7303=AXIS2_PLACEMENT_3D('',#12407,#8800,#8801);
#7304=AXIS2_PLACEMENT_3D('',#12413,#8805,#8806);
#7305=AXIS2_PLACEMENT_3D('',#12419,#8810,#8811);
#7306=AXIS2_PLACEMENT_3D('',#12422,#8814,#8815);
#7307=AXIS2_PLACEMENT_3D('',#12423,#8816,#8817);
#7308=AXIS2_PLACEMENT_3D('',#12424,#8818,#8819);
#7309=AXIS2_PLACEMENT_3D('',#12425,#8820,#8821);
#7310=AXIS2_PLACEMENT_3D('',#12426,#8822,#8823);
#7311=AXIS2_PLACEMENT_3D('',#12429,#8824,#8825);
#7312=AXIS2_PLACEMENT_3D('',#12435,#8829,#8830);
#7313=AXIS2_PLACEMENT_3D('',#12441,#8834,#8835);
#7314=AXIS2_PLACEMENT_3D('',#12443,#8836,#8837);
#7315=AXIS2_PLACEMENT_3D('',#12447,#8840,#8841);
#7316=AXIS2_PLACEMENT_3D('',#12450,#8844,#8845);
#7317=AXIS2_PLACEMENT_3D('',#12451,#8846,#8847);
#7318=AXIS2_PLACEMENT_3D('',#12453,#8848,#8849);
#7319=AXIS2_PLACEMENT_3D('',#12455,#8850,#8851);
#7320=AXIS2_PLACEMENT_3D('',#12456,#8852,#8853);
#7321=AXIS2_PLACEMENT_3D('',#12458,#8854,#8855);
#7322=AXIS2_PLACEMENT_3D('',#12460,#8857,#8858);
#7323=AXIS2_PLACEMENT_3D('',#12462,#8859,#8860);
#7324=AXIS2_PLACEMENT_3D('',#12463,#8861,#8862);
#7325=AXIS2_PLACEMENT_3D('',#12465,#8863,#8864);
#7326=AXIS2_PLACEMENT_3D('',#12467,#8866,#8867);
#7327=AXIS2_PLACEMENT_3D('',#12469,#8868,#8869);
#7328=AXIS2_PLACEMENT_3D('',#12470,#8870,#8871);
#7329=AXIS2_PLACEMENT_3D('',#12472,#8872,#8873);
#7330=AXIS2_PLACEMENT_3D('',#12474,#8875,#8876);
#7331=AXIS2_PLACEMENT_3D('',#12476,#8877,#8878);
#7332=AXIS2_PLACEMENT_3D('',#12477,#8879,#8880);
#7333=AXIS2_PLACEMENT_3D('',#12479,#8881,#8882);
#7334=AXIS2_PLACEMENT_3D('',#12481,#8884,#8885);
#7335=AXIS2_PLACEMENT_3D('',#12483,#8886,#8887);
#7336=AXIS2_PLACEMENT_3D('',#12484,#8888,#8889);
#7337=AXIS2_PLACEMENT_3D('',#12486,#8890,#8891);
#7338=AXIS2_PLACEMENT_3D('',#12488,#8893,#8894);
#7339=AXIS2_PLACEMENT_3D('',#12490,#8895,#8896);
#7340=AXIS2_PLACEMENT_3D('',#12491,#8897,#8898);
#7341=AXIS2_PLACEMENT_3D('',#12493,#8900,#8901);
#7342=AXIS2_PLACEMENT_3D('',#12494,#8902,#8903);
#7343=AXIS2_PLACEMENT_3D('',#12497,#8904,#8905);
#7344=AXIS2_PLACEMENT_3D('',#12501,#8907,#8908);
#7345=AXIS2_PLACEMENT_3D('',#12503,#8910,#8911);
#7346=AXIS2_PLACEMENT_3D('',#12509,#8915,#8916);
#7347=AXIS2_PLACEMENT_3D('',#12511,#8917,#8918);
#7348=AXIS2_PLACEMENT_3D('',#12513,#8919,#8920);
#7349=AXIS2_PLACEMENT_3D('',#12515,#8922,#8923);
#7350=AXIS2_PLACEMENT_3D('',#12518,#8926,#8927);
#7351=AXIS2_PLACEMENT_3D('',#12520,#8928,#8929);
#7352=AXIS2_PLACEMENT_3D('',#12522,#8930,#8931);
#7353=AXIS2_PLACEMENT_3D('',#12523,#8932,#8933);
#7354=AXIS2_PLACEMENT_3D('',#12525,#8934,#8935);
#7355=AXIS2_PLACEMENT_3D('',#12527,#8937,#8938);
#7356=AXIS2_PLACEMENT_3D('',#12529,#8939,#8940);
#7357=AXIS2_PLACEMENT_3D('',#12530,#8941,#8942);
#7358=AXIS2_PLACEMENT_3D('',#12532,#8944,#8945);
#7359=AXIS2_PLACEMENT_3D('',#12533,#8946,#8947);
#7360=AXIS2_PLACEMENT_3D('',#12534,#8948,#8949);
#7361=AXIS2_PLACEMENT_3D('',#12535,#8950,#8951);
#7362=AXIS2_PLACEMENT_3D('',#12544,#8956,#8957);
#7363=AXIS2_PLACEMENT_3D('',#12550,#8961,#8962);
#7364=AXIS2_PLACEMENT_3D('',#12556,#8966,#8967);
#7365=AXIS2_PLACEMENT_3D('',#12562,#8971,#8972);
#7366=AXIS2_PLACEMENT_3D('',#12568,#8976,#8977);
#7367=AXIS2_PLACEMENT_3D('',#12571,#8980,#8981);
#7368=AXIS2_PLACEMENT_3D('',#12572,#8982,#8983);
#7369=AXIS2_PLACEMENT_3D('',#12573,#8984,#8985);
#7370=AXIS2_PLACEMENT_3D('',#12575,#8986,#8987);
#7371=AXIS2_PLACEMENT_3D('',#12576,#8988,#8989);
#7372=AXIS2_PLACEMENT_3D('',#12578,#8990,#8991);
#7373=AXIS2_PLACEMENT_3D('',#12579,#8992,#8993);
#7374=AXIS2_PLACEMENT_3D('',#12581,#8994,#8995);
#7375=AXIS2_PLACEMENT_3D('',#12583,#8997,#8998);
#7376=AXIS2_PLACEMENT_3D('',#12585,#8999,#9000);
#7377=AXIS2_PLACEMENT_3D('',#12587,#9002,#9003);
#7378=AXIS2_PLACEMENT_3D('',#12589,#9004,#9005);
#7379=AXIS2_PLACEMENT_3D('',#12591,#9007,#9008);
#7380=AXIS2_PLACEMENT_3D('',#12593,#9009,#9010);
#7381=AXIS2_PLACEMENT_3D('',#12594,#9011,#9012);
#7382=AXIS2_PLACEMENT_3D('',#12596,#9013,#9014);
#7383=AXIS2_PLACEMENT_3D('',#12598,#9016,#9017);
#7384=AXIS2_PLACEMENT_3D('',#12600,#9019,#9020);
#7385=AXIS2_PLACEMENT_3D('',#12601,#9021,#9022);
#7386=AXIS2_PLACEMENT_3D('',#12602,#9023,#9024);
#7387=AXIS2_PLACEMENT_3D('',#12604,#9025,#9026);
#7388=AXIS2_PLACEMENT_3D('',#12607,#9028,#9029);
#7389=AXIS2_PLACEMENT_3D('',#12608,#9030,#9031);
#7390=AXIS2_PLACEMENT_3D('',#12609,#9032,#9033);
#7391=AXIS2_PLACEMENT_3D('',#12611,#9034,#9035);
#7392=AXIS2_PLACEMENT_3D('',#12614,#9037,#9038);
#7393=AXIS2_PLACEMENT_3D('',#12615,#9039,#9040);
#7394=AXIS2_PLACEMENT_3D('',#12616,#9041,#9042);
#7395=AXIS2_PLACEMENT_3D('',#12625,#9047,#9048);
#7396=AXIS2_PLACEMENT_3D('',#12627,#9049,#9050);
#7397=AXIS2_PLACEMENT_3D('',#12631,#9053,#9054);
#7398=AXIS2_PLACEMENT_3D('',#12637,#9058,#9059);
#7399=AXIS2_PLACEMENT_3D('',#12639,#9061,#9062);
#7400=AXIS2_PLACEMENT_3D('',#12640,#9063,#9064);
#7401=AXIS2_PLACEMENT_3D('',#12641,#9065,#9066);
#7402=AXIS2_PLACEMENT_3D('',#12650,#9071,#9072);
#7403=AXIS2_PLACEMENT_3D('',#12652,#9073,#9074);
#7404=AXIS2_PLACEMENT_3D('',#12656,#9077,#9078);
#7405=AXIS2_PLACEMENT_3D('',#12662,#9082,#9083);
#7406=AXIS2_PLACEMENT_3D('',#12664,#9085,#9086);
#7407=AXIS2_PLACEMENT_3D('',#12665,#9087,#9088);
#7408=AXIS2_PLACEMENT_3D('',#12666,#9089,#9090);
#7409=AXIS2_PLACEMENT_3D('',#12668,#9091,#9092);
#7410=AXIS2_PLACEMENT_3D('',#12671,#9094,#9095);
#7411=AXIS2_PLACEMENT_3D('',#12672,#9096,#9097);
#7412=AXIS2_PLACEMENT_3D('',#12673,#9098,#9099);
#7413=AXIS2_PLACEMENT_3D('',#12674,#9100,#9101);
#7414=AXIS2_PLACEMENT_3D('',#12675,#9102,#9103);
#7415=AXIS2_PLACEMENT_3D('',#12677,#9104,#9105);
#7416=AXIS2_PLACEMENT_3D('',#12680,#9107,#9108);
#7417=AXIS2_PLACEMENT_3D('',#12681,#9109,#9110);
#7418=AXIS2_PLACEMENT_3D('',#12683,#9111,#9112);
#7419=AXIS2_PLACEMENT_3D('',#12686,#9114,#9115);
#7420=AXIS2_PLACEMENT_3D('',#12687,#9116,#9117);
#7421=AXIS2_PLACEMENT_3D('',#12688,#9118,#9119);
#7422=AXIS2_PLACEMENT_3D('',#12689,#9120,#9121);
#7423=AXIS2_PLACEMENT_3D('',#12690,#9122,#9123);
#7424=AXIS2_PLACEMENT_3D('',#12692,#9124,#9125);
#7425=AXIS2_PLACEMENT_3D('',#12695,#9127,#9128);
#7426=AXIS2_PLACEMENT_3D('',#12696,#9129,#9130);
#7427=AXIS2_PLACEMENT_3D('',#12698,#9131,#9132);
#7428=AXIS2_PLACEMENT_3D('',#12701,#9134,#9135);
#7429=AXIS2_PLACEMENT_3D('',#12702,#9136,#9137);
#7430=AXIS2_PLACEMENT_3D('',#12703,#9138,#9139);
#7431=AXIS2_PLACEMENT_3D('',#12704,#9140,#9141);
#7432=AXIS2_PLACEMENT_3D('',#12705,#9142,#9143);
#7433=AXIS2_PLACEMENT_3D('',#12707,#9144,#9145);
#7434=AXIS2_PLACEMENT_3D('',#12710,#9147,#9148);
#7435=AXIS2_PLACEMENT_3D('',#12711,#9149,#9150);
#7436=AXIS2_PLACEMENT_3D('',#12713,#9151,#9152);
#7437=AXIS2_PLACEMENT_3D('',#12716,#9154,#9155);
#7438=AXIS2_PLACEMENT_3D('',#12717,#9156,#9157);
#7439=AXIS2_PLACEMENT_3D('',#12718,#9158,#9159);
#7440=AXIS2_PLACEMENT_3D('',#12719,#9160,#9161);
#7441=AXIS2_PLACEMENT_3D('',#12720,#9162,#9163);
#7442=AXIS2_PLACEMENT_3D('',#12722,#9164,#9165);
#7443=AXIS2_PLACEMENT_3D('',#12725,#9167,#9168);
#7444=AXIS2_PLACEMENT_3D('',#12726,#9169,#9170);
#7445=AXIS2_PLACEMENT_3D('',#12728,#9171,#9172);
#7446=AXIS2_PLACEMENT_3D('',#12731,#9174,#9175);
#7447=AXIS2_PLACEMENT_3D('',#12732,#9176,#9177);
#7448=AXIS2_PLACEMENT_3D('',#12733,#9178,#9179);
#7449=AXIS2_PLACEMENT_3D('',#12734,#9180,#9181);
#7450=AXIS2_PLACEMENT_3D('',#12735,#9182,#9183);
#7451=AXIS2_PLACEMENT_3D('',#12744,#9188,#9189);
#7452=AXIS2_PLACEMENT_3D('',#12750,#9193,#9194);
#7453=AXIS2_PLACEMENT_3D('',#12756,#9198,#9199);
#7454=AXIS2_PLACEMENT_3D('',#12758,#9200,#9201);
#7455=AXIS2_PLACEMENT_3D('',#12759,#9202,#9203);
#7456=AXIS2_PLACEMENT_3D('',#12760,#9204,#9205);
#7457=AXIS2_PLACEMENT_3D('',#12761,#9206,#9207);
#7458=AXIS2_PLACEMENT_3D('',#12762,#9208,#9209);
#7459=AXIS2_PLACEMENT_3D('',#12764,#9210,#9211);
#7460=AXIS2_PLACEMENT_3D('',#12767,#9213,#9214);
#7461=AXIS2_PLACEMENT_3D('',#12768,#9215,#9216);
#7462=AXIS2_PLACEMENT_3D('',#12771,#9218,#9219);
#7463=AXIS2_PLACEMENT_3D('',#12772,#9220,#9221);
#7464=AXIS2_PLACEMENT_3D('',#12773,#9222,#9223);
#7465=AXIS2_PLACEMENT_3D('',#12775,#9224,#9225);
#7466=AXIS2_PLACEMENT_3D('',#12778,#9227,#9228);
#7467=AXIS2_PLACEMENT_3D('',#12779,#9229,#9230);
#7468=AXIS2_PLACEMENT_3D('',#12780,#9231,#9232);
#7469=AXIS2_PLACEMENT_3D('',#12781,#9233,#9234);
#7470=AXIS2_PLACEMENT_3D('',#12782,#9235,#9236);
#7471=AXIS2_PLACEMENT_3D('',#12784,#9237,#9238);
#7472=AXIS2_PLACEMENT_3D('',#12787,#9240,#9241);
#7473=AXIS2_PLACEMENT_3D('',#12788,#9242,#9243);
#7474=AXIS2_PLACEMENT_3D('',#12797,#9248,#9249);
#7475=AXIS2_PLACEMENT_3D('',#12803,#9253,#9254);
#7476=AXIS2_PLACEMENT_3D('',#12809,#9258,#9259);
#7477=AXIS2_PLACEMENT_3D('',#12811,#9260,#9261);
#7478=AXIS2_PLACEMENT_3D('',#12812,#9262,#9263);
#7479=AXIS2_PLACEMENT_3D('',#12813,#9264,#9265);
#7480=AXIS2_PLACEMENT_3D('',#12814,#9266,#9267);
#7481=AXIS2_PLACEMENT_3D('',#12815,#9268,#9269);
#7482=AXIS2_PLACEMENT_3D('',#12820,#9271,#9272);
#7483=AXIS2_PLACEMENT_3D('',#12823,#9274,#9275);
#7484=AXIS2_PLACEMENT_3D('',#12824,#9276,#9277);
#7485=AXIS2_PLACEMENT_3D('',#12828,#9279,#9280);
#7486=AXIS2_PLACEMENT_3D('',#12830,#9282,#9283);
#7487=AXIS2_PLACEMENT_3D('',#12834,#9286,#9287);
#7488=AXIS2_PLACEMENT_3D('',#12838,#9290,#9291);
#7489=AXIS2_PLACEMENT_3D('',#12839,#9292,#9293);
#7490=AXIS2_PLACEMENT_3D('',#12840,#9294,#9295);
#7491=AXIS2_PLACEMENT_3D('',#12843,#9297,#9298);
#7492=AXIS2_PLACEMENT_3D('',#12844,#9299,#9300);
#7493=AXIS2_PLACEMENT_3D('',#12845,#9301,#9302);
#7494=AXIS2_PLACEMENT_3D('',#12846,#9303,#9304);
#7495=AXIS2_PLACEMENT_3D('',#12848,#9305,#9306);
#7496=AXIS2_PLACEMENT_3D('',#12851,#9308,#9309);
#7497=AXIS2_PLACEMENT_3D('',#12852,#9310,#9311);
#7498=AXIS2_PLACEMENT_3D('',#12853,#9312,#9313);
#7499=AXIS2_PLACEMENT_3D('',#12855,#9314,#9315);
#7500=AXIS2_PLACEMENT_3D('',#12858,#9317,#9318);
#7501=AXIS2_PLACEMENT_3D('',#12859,#9319,#9320);
#7502=AXIS2_PLACEMENT_3D('',#12860,#9321,#9322);
#7503=AXIS2_PLACEMENT_3D('',#12861,#9323,#9324);
#7504=AXIS2_PLACEMENT_3D('',#12862,#9325,#9326);
#7505=AXIS2_PLACEMENT_3D('',#12864,#9327,#9328);
#7506=AXIS2_PLACEMENT_3D('',#12867,#9330,#9331);
#7507=AXIS2_PLACEMENT_3D('',#12868,#9332,#9333);
#7508=AXIS2_PLACEMENT_3D('',#12870,#9334,#9335);
#7509=AXIS2_PLACEMENT_3D('',#12873,#9337,#9338);
#7510=AXIS2_PLACEMENT_3D('',#12874,#9339,#9340);
#7511=AXIS2_PLACEMENT_3D('',#12875,#9341,#9342);
#7512=AXIS2_PLACEMENT_3D('',#12876,#9343,#9344);
#7513=AXIS2_PLACEMENT_3D('',#12877,#9345,#9346);
#7514=AXIS2_PLACEMENT_3D('',#12879,#9347,#9348);
#7515=AXIS2_PLACEMENT_3D('',#12882,#9350,#9351);
#7516=AXIS2_PLACEMENT_3D('',#12883,#9352,#9353);
#7517=AXIS2_PLACEMENT_3D('',#12885,#9354,#9355);
#7518=AXIS2_PLACEMENT_3D('',#12888,#9357,#9358);
#7519=AXIS2_PLACEMENT_3D('',#12889,#9359,#9360);
#7520=AXIS2_PLACEMENT_3D('',#12890,#9361,#9362);
#7521=AXIS2_PLACEMENT_3D('',#12891,#9363,#9364);
#7522=AXIS2_PLACEMENT_3D('',#12892,#9365,#9366);
#7523=AXIS2_PLACEMENT_3D('',#12909,#9375,#9376);
#7524=AXIS2_PLACEMENT_3D('',#12915,#9380,#9381);
#7525=AXIS2_PLACEMENT_3D('',#12919,#9384,#9385);
#7526=AXIS2_PLACEMENT_3D('',#12923,#9388,#9389);
#7527=AXIS2_PLACEMENT_3D('',#12927,#9392,#9393);
#7528=AXIS2_PLACEMENT_3D('',#12935,#9398,#9399);
#7529=AXIS2_PLACEMENT_3D('',#12937,#9401,#9402);
#7530=AXIS2_PLACEMENT_3D('',#12939,#9404,#9405);
#7531=AXIS2_PLACEMENT_3D('',#12941,#9407,#9408);
#7532=AXIS2_PLACEMENT_3D('',#12942,#9409,#9410);
#7533=AXIS2_PLACEMENT_3D('',#12943,#9411,#9412);
#7534=AXIS2_PLACEMENT_3D('',#12945,#9413,#9414);
#7535=AXIS2_PLACEMENT_3D('',#12946,#9415,#9416);
#7536=AXIS2_PLACEMENT_3D('',#12948,#9417,#9418);
#7537=AXIS2_PLACEMENT_3D('',#12950,#9420,#9421);
#7538=AXIS2_PLACEMENT_3D('',#12952,#9422,#9423);
#7539=AXIS2_PLACEMENT_3D('',#12954,#9425,#9426);
#7540=AXIS2_PLACEMENT_3D('',#12956,#9427,#9428);
#7541=AXIS2_PLACEMENT_3D('',#12958,#9430,#9431);
#7542=AXIS2_PLACEMENT_3D('',#12960,#9432,#9433);
#7543=AXIS2_PLACEMENT_3D('',#12961,#9434,#9435);
#7544=AXIS2_PLACEMENT_3D('',#12963,#9436,#9437);
#7545=AXIS2_PLACEMENT_3D('',#12965,#9439,#9440);
#7546=AXIS2_PLACEMENT_3D('',#12967,#9441,#9442);
#7547=AXIS2_PLACEMENT_3D('',#12969,#9444,#9445);
#7548=AXIS2_PLACEMENT_3D('',#12971,#9446,#9447);
#7549=AXIS2_PLACEMENT_3D('',#12973,#9449,#9450);
#7550=AXIS2_PLACEMENT_3D('',#12974,#9451,#9452);
#7551=AXIS2_PLACEMENT_3D('',#12983,#9457,#9458);
#7552=AXIS2_PLACEMENT_3D('',#12989,#9462,#9463);
#7553=AXIS2_PLACEMENT_3D('',#12995,#9467,#9468);
#7554=AXIS2_PLACEMENT_3D('',#13001,#9472,#9473);
#7555=AXIS2_PLACEMENT_3D('',#13007,#9477,#9478);
#7556=AXIS2_PLACEMENT_3D('',#13010,#9481,#9482);
#7557=AXIS2_PLACEMENT_3D('',#13011,#9483,#9484);
#7558=AXIS2_PLACEMENT_3D('',#13012,#9485,#9486);
#7559=AXIS2_PLACEMENT_3D('',#13013,#9487,#9488);
#7560=AXIS2_PLACEMENT_3D('',#13014,#9489,#9490);
#7561=AXIS2_PLACEMENT_3D('',#13015,#9491,#9492);
#7562=AXIS2_PLACEMENT_3D('',#13016,#9493,#9494);
#7563=AXIS2_PLACEMENT_3D('',#13017,#9495,#9496);
#7564=AXIS2_PLACEMENT_3D('',#13018,#9497,#9498);
#7565=AXIS2_PLACEMENT_3D('',#13019,#9499,#9500);
#7566=AXIS2_PLACEMENT_3D('',#13020,#9501,#9502);
#7567=AXIS2_PLACEMENT_3D('',#13021,#9503,#9504);
#7568=AXIS2_PLACEMENT_3D('',#13022,#9505,#9506);
#7569=AXIS2_PLACEMENT_3D('',#13023,#9507,#9508);
#7570=AXIS2_PLACEMENT_3D('',#13024,#9509,#9510);
#7571=AXIS2_PLACEMENT_3D('',#13025,#9511,#9512);
#7572=AXIS2_PLACEMENT_3D('',#13026,#9513,#9514);
#7573=AXIS2_PLACEMENT_3D('',#13027,#9515,#9516);
#7574=AXIS2_PLACEMENT_3D('',#13028,#9517,#9518);
#7575=AXIS2_PLACEMENT_3D('',#13029,#9519,#9520);
#7576=AXIS2_PLACEMENT_3D('',#13030,#9521,#9522);
#7577=AXIS2_PLACEMENT_3D('',#13031,#9523,#9524);
#7578=AXIS2_PLACEMENT_3D('',#13032,#9525,#9526);
#7579=AXIS2_PLACEMENT_3D('',#13033,#9527,#9528);
#7580=AXIS2_PLACEMENT_3D('',#13034,#9529,#9530);
#7581=AXIS2_PLACEMENT_3D('',#13035,#9531,#9532);
#7582=AXIS2_PLACEMENT_3D('',#13036,#9533,#9534);
#7583=AXIS2_PLACEMENT_3D('',#13037,#9535,#9536);
#7584=AXIS2_PLACEMENT_3D('',#13038,#9537,#9538);
#7585=AXIS2_PLACEMENT_3D('',#13039,#9539,#9540);
#7586=AXIS2_PLACEMENT_3D('',#13040,#9541,#9542);
#7587=AXIS2_PLACEMENT_3D('',#13041,#9543,#9544);
#7588=AXIS2_PLACEMENT_3D('',#13042,#9545,#9546);
#7589=AXIS2_PLACEMENT_3D('',#13043,#9547,#9548);
#7590=AXIS2_PLACEMENT_3D('',#13044,#9549,#9550);
#7591=AXIS2_PLACEMENT_3D('',#13045,#9551,#9552);
#7592=AXIS2_PLACEMENT_3D('',#13046,#9553,#9554);
#7593=AXIS2_PLACEMENT_3D('',#13047,#9555,#9556);
#7594=AXIS2_PLACEMENT_3D('',#13048,#9557,#9558);
#7595=AXIS2_PLACEMENT_3D('',#13049,#9559,#9560);
#7596=AXIS2_PLACEMENT_3D('',#13050,#9561,#9562);
#7597=AXIS2_PLACEMENT_3D('',#13051,#9563,#9564);
#7598=AXIS2_PLACEMENT_3D('',#13052,#9565,#9566);
#7599=AXIS2_PLACEMENT_3D('',#13053,#9567,#9568);
#7600=AXIS2_PLACEMENT_3D('',#13054,#9569,#9570);
#7601=AXIS2_PLACEMENT_3D('',#13055,#9571,#9572);
#7602=AXIS2_PLACEMENT_3D('',#13056,#9573,#9574);
#7603=AXIS2_PLACEMENT_3D('',#13057,#9575,#9576);
#7604=AXIS2_PLACEMENT_3D('',#13058,#9577,#9578);
#7605=AXIS2_PLACEMENT_3D('',#13059,#9579,#9580);
#7606=AXIS2_PLACEMENT_3D('',#13060,#9581,#9582);
#7607=AXIS2_PLACEMENT_3D('',#13061,#9583,#9584);
#7608=AXIS2_PLACEMENT_3D('',#13062,#9585,#9586);
#7609=AXIS2_PLACEMENT_3D('',#13063,#9587,#9588);
#7610=AXIS2_PLACEMENT_3D('',#13064,#9589,#9590);
#7611=AXIS2_PLACEMENT_3D('',#13065,#9591,#9592);
#7612=AXIS2_PLACEMENT_3D('',#13066,#9593,#9594);
#7613=AXIS2_PLACEMENT_3D('',#13067,#9595,#9596);
#7614=AXIS2_PLACEMENT_3D('',#13068,#9597,#9598);
#7615=AXIS2_PLACEMENT_3D('',#13069,#9599,#9600);
#7616=AXIS2_PLACEMENT_3D('',#13070,#9601,#9602);
#7617=AXIS2_PLACEMENT_3D('',#13071,#9603,#9604);
#7618=AXIS2_PLACEMENT_3D('',#13072,#9605,#9606);
#7619=AXIS2_PLACEMENT_3D('',#13074,#9607,#9608);
#7620=AXIS2_PLACEMENT_3D('',#13077,#9610,#9611);
#7621=AXIS2_PLACEMENT_3D('',#13078,#9612,#9613);
#7622=AXIS2_PLACEMENT_3D('',#13087,#9618,#9619);
#7623=AXIS2_PLACEMENT_3D('',#13093,#9623,#9624);
#7624=AXIS2_PLACEMENT_3D('',#13099,#9628,#9629);
#7625=AXIS2_PLACEMENT_3D('',#13102,#9632,#9633);
#7626=AXIS2_PLACEMENT_3D('',#13103,#9634,#9635);
#7627=AXIS2_PLACEMENT_3D('',#13104,#9636,#9637);
#7628=AXIS2_PLACEMENT_3D('',#13105,#9638,#9639);
#7629=AXIS2_PLACEMENT_3D('',#13107,#9640,#9641);
#7630=AXIS2_PLACEMENT_3D('',#13110,#9643,#9644);
#7631=AXIS2_PLACEMENT_3D('',#13111,#9645,#9646);
#7632=AXIS2_PLACEMENT_3D('',#13113,#9647,#9648);
#7633=AXIS2_PLACEMENT_3D('',#13116,#9650,#9651);
#7634=AXIS2_PLACEMENT_3D('',#13117,#9652,#9653);
#7635=AXIS2_PLACEMENT_3D('',#13119,#9654,#9655);
#7636=AXIS2_PLACEMENT_3D('',#13122,#9657,#9658);
#7637=AXIS2_PLACEMENT_3D('',#13123,#9659,#9660);
#7638=AXIS2_PLACEMENT_3D('',#13125,#9661,#9662);
#7639=AXIS2_PLACEMENT_3D('',#13128,#9664,#9665);
#7640=AXIS2_PLACEMENT_3D('',#13129,#9666,#9667);
#7641=AXIS2_PLACEMENT_3D('',#13139,#9672,#9673);
#7642=AXIS2_PLACEMENT_3D('',#13140,#9674,#9675);
#7643=AXIS2_PLACEMENT_3D('',#13146,#9679,#9680);
#7644=AXIS2_PLACEMENT_3D('',#13150,#9683,#9684);
#7645=AXIS2_PLACEMENT_3D('',#13154,#9687,#9688);
#7646=AXIS2_PLACEMENT_3D('',#13156,#9690,#9691);
#7647=AXIS2_PLACEMENT_3D('',#13157,#9692,#9693);
#7648=AXIS2_PLACEMENT_3D('',#13159,#9694,#9695);
#7649=AXIS2_PLACEMENT_3D('',#13162,#9697,#9698);
#7650=AXIS2_PLACEMENT_3D('',#13163,#9699,#9700);
#7651=AXIS2_PLACEMENT_3D('',#13164,#9701,#9702);
#7652=AXIS2_PLACEMENT_3D('',#13167,#9704,#9705);
#7653=AXIS2_PLACEMENT_3D('',#13168,#9706,#9707);
#7654=AXIS2_PLACEMENT_3D('',#13169,#9708,#9709);
#7655=AXIS2_PLACEMENT_3D('',#13170,#9710,#9711);
#7656=AXIS2_PLACEMENT_3D('',#13172,#9712,#9713);
#7657=AXIS2_PLACEMENT_3D('',#13175,#9715,#9716);
#7658=AXIS2_PLACEMENT_3D('',#13176,#9717,#9718);
#7659=AXIS2_PLACEMENT_3D('',#13178,#9719,#9720);
#7660=AXIS2_PLACEMENT_3D('',#13181,#9722,#9723);
#7661=AXIS2_PLACEMENT_3D('',#13182,#9724,#9725);
#7662=AXIS2_PLACEMENT_3D('',#13183,#9726,#9727);
#7663=AXIS2_PLACEMENT_3D('',#13184,#9728,#9729);
#7664=AXIS2_PLACEMENT_3D('',#13185,#9730,#9731);
#7665=AXIS2_PLACEMENT_3D('',#13186,#9732,#9733);
#7666=AXIS2_PLACEMENT_3D('',#13187,#9734,#9735);
#7667=AXIS2_PLACEMENT_3D('',#13188,#9736,#9737);
#7668=AXIS2_PLACEMENT_3D('',#13189,#9738,#9739);
#7669=DIRECTION('axis',(0.,0.,1.));
#7670=DIRECTION('refdir',(1.,0.,0.));
#7671=DIRECTION('axis',(0.,0.,1.));
#7672=DIRECTION('refdir',(1.,0.,0.));
#7673=DIRECTION('axis',(0.,0.,1.));
#7674=DIRECTION('refdir',(1.,0.,0.));
#7675=DIRECTION('center_axis',(0.,0.,1.));
#7676=DIRECTION('ref_axis',(1.,0.,0.));
#7677=DIRECTION('center_axis',(0.,0.,1.));
#7678=DIRECTION('ref_axis',(1.,0.,0.));
#7679=DIRECTION('',(0.,0.,1.));
#7680=DIRECTION('center_axis',(0.,0.,-1.));
#7681=DIRECTION('ref_axis',(1.,0.,0.));
#7682=DIRECTION('center_axis',(0.,0.,1.));
#7683=DIRECTION('ref_axis',(1.,0.,0.));
#7684=DIRECTION('center_axis',(0.,0.,1.));
#7685=DIRECTION('ref_axis',(1.,0.,0.));
#7686=DIRECTION('',(0.,0.,1.));
#7687=DIRECTION('center_axis',(0.,0.,-1.));
#7688=DIRECTION('ref_axis',(1.,0.,0.));
#7689=DIRECTION('center_axis',(0.,0.,1.));
#7690=DIRECTION('ref_axis',(1.,0.,0.));
#7691=DIRECTION('center_axis',(0.,0.,1.));
#7692=DIRECTION('ref_axis',(1.,0.,0.));
#7693=DIRECTION('',(0.,0.,1.));
#7694=DIRECTION('center_axis',(0.,0.,-1.));
#7695=DIRECTION('ref_axis',(1.,0.,0.));
#7696=DIRECTION('center_axis',(0.,0.,1.));
#7697=DIRECTION('ref_axis',(1.,0.,0.));
#7698=DIRECTION('center_axis',(0.,0.,1.));
#7699=DIRECTION('ref_axis',(1.,0.,0.));
#7700=DIRECTION('',(0.,0.,1.));
#7701=DIRECTION('center_axis',(0.,0.,-1.));
#7702=DIRECTION('ref_axis',(1.,0.,0.));
#7703=DIRECTION('center_axis',(0.,0.,1.));
#7704=DIRECTION('ref_axis',(1.,0.,0.));
#7705=DIRECTION('center_axis',(0.,0.,1.));
#7706=DIRECTION('ref_axis',(1.,0.,0.));
#7707=DIRECTION('',(0.,0.,1.));
#7708=DIRECTION('center_axis',(0.,0.,-1.));
#7709=DIRECTION('ref_axis',(1.,0.,0.));
#7710=DIRECTION('center_axis',(0.,0.,1.));
#7711=DIRECTION('ref_axis',(1.,0.,0.));
#7712=DIRECTION('center_axis',(0.,0.,1.));
#7713=DIRECTION('ref_axis',(1.,0.,0.));
#7714=DIRECTION('',(0.,0.,1.));
#7715=DIRECTION('center_axis',(0.,0.,-1.));
#7716=DIRECTION('ref_axis',(1.,0.,0.));
#7717=DIRECTION('center_axis',(0.,-1.,0.));
#7718=DIRECTION('ref_axis',(1.,0.,0.));
#7719=DIRECTION('',(-1.,0.,0.));
#7720=DIRECTION('',(0.,0.,1.));
#7721=DIRECTION('',(1.,0.,0.));
#7722=DIRECTION('',(0.,0.,1.));
#7723=DIRECTION('center_axis',(-1.,0.,0.));
#7724=DIRECTION('ref_axis',(0.,-1.,0.));
#7725=DIRECTION('',(0.,1.,0.));
#7726=DIRECTION('',(0.,-1.,0.));
#7727=DIRECTION('',(0.,0.,1.));
#7728=DIRECTION('center_axis',(0.,1.,0.));
#7729=DIRECTION('ref_axis',(-1.,0.,0.));
#7730=DIRECTION('',(1.,0.,0.));
#7731=DIRECTION('',(-1.,0.,0.));
#7732=DIRECTION('',(0.,0.,1.));
#7733=DIRECTION('center_axis',(1.,0.,0.));
#7734=DIRECTION('ref_axis',(0.,1.,0.));
#7735=DIRECTION('',(0.,-1.,0.));
#7736=DIRECTION('',(0.,1.,0.));
#7737=DIRECTION('center_axis',(0.,0.,1.));
#7738=DIRECTION('ref_axis',(1.,0.,0.));
#7739=DIRECTION('center_axis',(0.,1.,0.));
#7740=DIRECTION('ref_axis',(-1.,0.,0.));
#7741=DIRECTION('',(-1.,0.,0.));
#7742=DIRECTION('',(0.,0.,1.));
#7743=DIRECTION('',(-1.,0.,0.));
#7744=DIRECTION('',(0.,0.,1.));
#7745=DIRECTION('center_axis',(1.,0.,0.));
#7746=DIRECTION('ref_axis',(0.,1.,0.));
#7747=DIRECTION('',(0.,1.,0.));
#7748=DIRECTION('',(0.,1.,0.));
#7749=DIRECTION('',(0.,0.,1.));
#7750=DIRECTION('center_axis',(0.,-1.,0.));
#7751=DIRECTION('ref_axis',(1.,0.,0.));
#7752=DIRECTION('',(1.,0.,0.));
#7753=DIRECTION('',(1.,0.,0.));
#7754=DIRECTION('',(0.,0.,1.));
#7755=DIRECTION('center_axis',(-1.,0.,0.));
#7756=DIRECTION('ref_axis',(0.,-1.,0.));
#7757=DIRECTION('',(0.,-1.,0.));
#7758=DIRECTION('',(0.,-1.,0.));
#7759=DIRECTION('center_axis',(0.,0.,1.));
#7760=DIRECTION('ref_axis',(1.,0.,0.));
#7761=DIRECTION('center_axis',(0.,0.,1.));
#7762=DIRECTION('ref_axis',(1.,0.,0.));
#7763=DIRECTION('axis',(0.,0.,1.));
#7764=DIRECTION('refdir',(1.,0.,0.));
#7765=DIRECTION('center_axis',(0.,1.,0.));
#7766=DIRECTION('ref_axis',(-1.,0.,0.));
#7767=DIRECTION('',(-1.,0.,0.));
#7768=DIRECTION('',(0.,0.,1.));
#7769=DIRECTION('',(-1.,0.,0.));
#7770=DIRECTION('',(0.,0.,1.));
#7771=DIRECTION('center_axis',(1.,0.,0.));
#7772=DIRECTION('ref_axis',(0.,1.,0.));
#7773=DIRECTION('',(0.,1.,0.));
#7774=DIRECTION('',(0.,1.,0.));
#7775=DIRECTION('',(0.,0.,1.));
#7776=DIRECTION('center_axis',(0.,-1.,0.));
#7777=DIRECTION('ref_axis',(1.,0.,0.));
#7778=DIRECTION('',(1.,0.,0.));
#7779=DIRECTION('',(1.,0.,0.));
#7780=DIRECTION('',(0.,0.,1.));
#7781=DIRECTION('center_axis',(-1.,0.,0.));
#7782=DIRECTION('ref_axis',(0.,-1.,0.));
#7783=DIRECTION('',(0.,-1.,0.));
#7784=DIRECTION('',(0.,-1.,0.));
#7785=DIRECTION('center_axis',(0.,0.,1.));
#7786=DIRECTION('ref_axis',(1.,0.,0.));
#7787=DIRECTION('center_axis',(0.,0.,1.));
#7788=DIRECTION('ref_axis',(1.,0.,0.));
#7789=DIRECTION('axis',(0.,0.,1.));
#7790=DIRECTION('refdir',(1.,0.,0.));
#7791=DIRECTION('center_axis',(0.,1.,0.));
#7792=DIRECTION('ref_axis',(-1.,0.,0.));
#7793=DIRECTION('',(-1.,0.,0.));
#7794=DIRECTION('',(0.,0.,1.));
#7795=DIRECTION('',(-1.,0.,0.));
#7796=DIRECTION('',(0.,0.,1.));
#7797=DIRECTION('center_axis',(1.,0.,0.));
#7798=DIRECTION('ref_axis',(0.,1.,0.));
#7799=DIRECTION('',(0.,1.,0.));
#7800=DIRECTION('',(0.,1.,0.));
#7801=DIRECTION('',(0.,0.,1.));
#7802=DIRECTION('center_axis',(0.,-1.,0.));
#7803=DIRECTION('ref_axis',(1.,0.,0.));
#7804=DIRECTION('',(1.,0.,0.));
#7805=DIRECTION('',(1.,0.,0.));
#7806=DIRECTION('',(0.,0.,1.));
#7807=DIRECTION('center_axis',(-1.,0.,0.));
#7808=DIRECTION('ref_axis',(0.,-1.,0.));
#7809=DIRECTION('',(0.,-1.,0.));
#7810=DIRECTION('',(0.,-1.,0.));
#7811=DIRECTION('center_axis',(0.,0.,1.));
#7812=DIRECTION('ref_axis',(1.,0.,0.));
#7813=DIRECTION('center_axis',(0.,0.,1.));
#7814=DIRECTION('ref_axis',(1.,0.,0.));
#7815=DIRECTION('axis',(0.,0.,1.));
#7816=DIRECTION('refdir',(1.,0.,0.));
#7817=DIRECTION('center_axis',(0.,0.,1.));
#7818=DIRECTION('ref_axis',(1.,0.,0.));
#7819=DIRECTION('center_axis',(0.,0.,1.));
#7820=DIRECTION('ref_axis',(1.,0.,0.));
#7821=DIRECTION('',(0.,0.,1.));
#7822=DIRECTION('center_axis',(0.,0.,-1.));
#7823=DIRECTION('ref_axis',(1.,0.,0.));
#7824=DIRECTION('center_axis',(0.,0.,1.));
#7825=DIRECTION('ref_axis',(1.,0.,0.));
#7826=DIRECTION('center_axis',(0.,0.,1.));
#7827=DIRECTION('ref_axis',(1.,0.,0.));
#7828=DIRECTION('',(0.,0.,1.));
#7829=DIRECTION('center_axis',(0.,0.,-1.));
#7830=DIRECTION('ref_axis',(1.,0.,0.));
#7831=DIRECTION('center_axis',(0.,1.,0.));
#7832=DIRECTION('ref_axis',(1.,0.,0.));
#7833=DIRECTION('center_axis',(0.,1.,0.));
#7834=DIRECTION('ref_axis',(1.,0.,0.));
#7835=DIRECTION('',(0.,1.,0.));
#7836=DIRECTION('center_axis',(0.,-1.,0.));
#7837=DIRECTION('ref_axis',(1.,0.,0.));
#7838=DIRECTION('center_axis',(0.,1.,0.));
#7839=DIRECTION('ref_axis',(1.,0.,0.));
#7840=DIRECTION('center_axis',(0.,1.,0.));
#7841=DIRECTION('ref_axis',(1.,0.,0.));
#7842=DIRECTION('',(0.,1.,0.));
#7843=DIRECTION('center_axis',(0.,-1.,0.));
#7844=DIRECTION('ref_axis',(1.,0.,0.));
#7845=DIRECTION('center_axis',(0.,1.,0.));
#7846=DIRECTION('ref_axis',(1.,0.,0.));
#7847=DIRECTION('center_axis',(0.,1.,0.));
#7848=DIRECTION('ref_axis',(1.,0.,0.));
#7849=DIRECTION('',(0.,1.,0.));
#7850=DIRECTION('center_axis',(0.,-1.,0.));
#7851=DIRECTION('ref_axis',(1.,0.,0.));
#7852=DIRECTION('center_axis',(0.,1.,0.));
#7853=DIRECTION('ref_axis',(1.,0.,0.));
#7854=DIRECTION('center_axis',(0.,1.,0.));
#7855=DIRECTION('ref_axis',(1.,0.,0.));
#7856=DIRECTION('',(0.,1.,0.));
#7857=DIRECTION('center_axis',(0.,-1.,0.));
#7858=DIRECTION('ref_axis',(1.,0.,0.));
#7859=DIRECTION('center_axis',(0.,1.,0.));
#7860=DIRECTION('ref_axis',(1.,0.,0.));
#7861=DIRECTION('center_axis',(0.,1.,0.));
#7862=DIRECTION('ref_axis',(1.,0.,0.));
#7863=DIRECTION('',(0.,1.,0.));
#7864=DIRECTION('center_axis',(0.,-1.,0.));
#7865=DIRECTION('ref_axis',(1.,0.,0.));
#7866=DIRECTION('center_axis',(0.,0.,1.));
#7867=DIRECTION('ref_axis',(1.,0.,0.));
#7868=DIRECTION('',(0.,1.,0.));
#7869=DIRECTION('',(-1.,0.,0.));
#7870=DIRECTION('',(0.,1.,0.));
#7871=DIRECTION('',(1.,0.,0.));
#7872=DIRECTION('center_axis',(0.,0.,1.));
#7873=DIRECTION('ref_axis',(1.,0.,0.));
#7874=DIRECTION('',(0.,-1.,0.));
#7875=DIRECTION('',(1.,0.,0.));
#7876=DIRECTION('',(0.,1.,0.));
#7877=DIRECTION('',(-1.,0.,0.));
#7878=DIRECTION('center_axis',(-1.,0.,0.));
#7879=DIRECTION('ref_axis',(0.,0.,1.));
#7880=DIRECTION('',(0.,0.,-1.));
#7881=DIRECTION('',(0.,0.,1.));
#7882=DIRECTION('',(0.,1.,0.));
#7883=DIRECTION('center_axis',(1.,0.,0.));
#7884=DIRECTION('ref_axis',(0.,0.,-1.));
#7885=DIRECTION('',(0.,0.,1.));
#7886=DIRECTION('',(0.,1.,0.));
#7887=DIRECTION('',(0.,0.,-1.));
#7888=DIRECTION('center_axis',(0.,-1.,0.));
#7889=DIRECTION('ref_axis',(1.,0.,0.));
#7890=DIRECTION('',(0.,0.,1.));
#7891=DIRECTION('',(1.,0.,0.));
#7892=DIRECTION('',(0.,0.,1.));
#7893=DIRECTION('',(1.,0.,0.));
#7894=DIRECTION('center_axis',(1.,0.,0.));
#7895=DIRECTION('ref_axis',(0.,1.,0.));
#7896=DIRECTION('',(0.,0.,1.));
#7897=DIRECTION('',(0.,1.,0.));
#7898=DIRECTION('center_axis',(0.,1.,0.));
#7899=DIRECTION('ref_axis',(-1.,0.,0.));
#7900=DIRECTION('',(0.,0.,1.));
#7901=DIRECTION('',(-1.,0.,0.));
#7902=DIRECTION('',(-1.,0.,0.));
#7903=DIRECTION('center_axis',(-1.,0.,0.));
#7904=DIRECTION('ref_axis',(0.,-1.,0.));
#7905=DIRECTION('',(0.,-1.,0.));
#7906=DIRECTION('center_axis',(0.,0.,1.));
#7907=DIRECTION('ref_axis',(1.,0.,0.));
#7908=DIRECTION('center_axis',(0.,0.,1.));
#7909=DIRECTION('ref_axis',(1.,0.,0.));
#7910=DIRECTION('axis',(0.,0.,1.));
#7911=DIRECTION('refdir',(1.,0.,0.));
#7912=DIRECTION('center_axis',(0.,1.,0.));
#7913=DIRECTION('ref_axis',(1.,0.,0.));
#7914=DIRECTION('center_axis',(0.,1.,0.));
#7915=DIRECTION('ref_axis',(1.,0.,0.));
#7916=DIRECTION('',(0.,1.,0.));
#7917=DIRECTION('center_axis',(0.,-1.,0.));
#7918=DIRECTION('ref_axis',(1.,0.,0.));
#7919=DIRECTION('center_axis',(0.,1.,0.));
#7920=DIRECTION('ref_axis',(1.,0.,0.));
#7921=DIRECTION('center_axis',(0.,1.,0.));
#7922=DIRECTION('ref_axis',(1.,0.,0.));
#7923=DIRECTION('',(0.,1.,0.));
#7924=DIRECTION('center_axis',(0.,-1.,0.));
#7925=DIRECTION('ref_axis',(1.,0.,0.));
#7926=DIRECTION('center_axis',(0.,1.,0.));
#7927=DIRECTION('ref_axis',(1.,0.,0.));
#7928=DIRECTION('center_axis',(0.,1.,0.));
#7929=DIRECTION('ref_axis',(1.,0.,0.));
#7930=DIRECTION('',(0.,1.,0.));
#7931=DIRECTION('center_axis',(0.,-1.,0.));
#7932=DIRECTION('ref_axis',(1.,0.,0.));
#7933=DIRECTION('center_axis',(0.,1.,0.));
#7934=DIRECTION('ref_axis',(1.,0.,0.));
#7935=DIRECTION('center_axis',(0.,1.,0.));
#7936=DIRECTION('ref_axis',(1.,0.,0.));
#7937=DIRECTION('',(0.,1.,0.));
#7938=DIRECTION('center_axis',(0.,-1.,0.));
#7939=DIRECTION('ref_axis',(1.,0.,0.));
#7940=DIRECTION('center_axis',(0.,1.,0.));
#7941=DIRECTION('ref_axis',(1.,0.,0.));
#7942=DIRECTION('center_axis',(0.,1.,0.));
#7943=DIRECTION('ref_axis',(1.,0.,0.));
#7944=DIRECTION('',(0.,-1.,0.));
#7945=DIRECTION('center_axis',(0.,-1.,0.));
#7946=DIRECTION('ref_axis',(1.,0.,0.));
#7947=DIRECTION('center_axis',(0.,1.,0.));
#7948=DIRECTION('ref_axis',(1.,0.,0.));
#7949=DIRECTION('center_axis',(0.,-1.,0.));
#7950=DIRECTION('ref_axis',(1.,0.,0.));
#7951=DIRECTION('center_axis',(0.,1.,0.));
#7952=DIRECTION('ref_axis',(1.,0.,0.));
#7953=DIRECTION('',(0.,-1.,0.));
#7954=DIRECTION('center_axis',(0.,-1.,0.));
#7955=DIRECTION('ref_axis',(1.,0.,0.));
#7956=DIRECTION('center_axis',(0.,1.,0.));
#7957=DIRECTION('ref_axis',(1.,0.,0.));
#7958=DIRECTION('center_axis',(0.,1.,0.));
#7959=DIRECTION('ref_axis',(1.,0.,0.));
#7960=DIRECTION('',(0.,-1.,0.));
#7961=DIRECTION('center_axis',(0.,1.,0.));
#7962=DIRECTION('ref_axis',(1.,0.,0.));
#7963=DIRECTION('center_axis',(0.,1.,0.));
#7964=DIRECTION('ref_axis',(1.,0.,0.));
#7965=DIRECTION('center_axis',(0.,1.,0.));
#7966=DIRECTION('ref_axis',(1.,0.,0.));
#7967=DIRECTION('axis',(0.,0.,1.));
#7968=DIRECTION('refdir',(1.,0.,0.));
#7969=DIRECTION('center_axis',(0.,1.,0.));
#7970=DIRECTION('ref_axis',(1.,0.,0.));
#7971=DIRECTION('center_axis',(0.,1.,0.));
#7972=DIRECTION('ref_axis',(1.,0.,0.));
#7973=DIRECTION('',(0.,1.,0.));
#7974=DIRECTION('center_axis',(0.,-1.,0.));
#7975=DIRECTION('ref_axis',(1.,0.,0.));
#7976=DIRECTION('center_axis',(0.,1.,0.));
#7977=DIRECTION('ref_axis',(1.,0.,0.));
#7978=DIRECTION('center_axis',(0.,1.,0.));
#7979=DIRECTION('ref_axis',(1.,0.,0.));
#7980=DIRECTION('',(0.,1.,0.));
#7981=DIRECTION('center_axis',(0.,-1.,0.));
#7982=DIRECTION('ref_axis',(1.,0.,0.));
#7983=DIRECTION('center_axis',(0.,1.,0.));
#7984=DIRECTION('ref_axis',(1.,0.,0.));
#7985=DIRECTION('center_axis',(0.,1.,0.));
#7986=DIRECTION('ref_axis',(1.,0.,0.));
#7987=DIRECTION('',(0.,1.,0.));
#7988=DIRECTION('center_axis',(0.,-1.,0.));
#7989=DIRECTION('ref_axis',(1.,0.,0.));
#7990=DIRECTION('center_axis',(0.,1.,0.));
#7991=DIRECTION('ref_axis',(1.,0.,0.));
#7992=DIRECTION('center_axis',(0.,1.,0.));
#7993=DIRECTION('ref_axis',(1.,0.,0.));
#7994=DIRECTION('',(0.,1.,0.));
#7995=DIRECTION('center_axis',(0.,-1.,0.));
#7996=DIRECTION('ref_axis',(1.,0.,0.));
#7997=DIRECTION('center_axis',(0.,1.,0.));
#7998=DIRECTION('ref_axis',(1.,0.,0.));
#7999=DIRECTION('center_axis',(0.,1.,0.));
#8000=DIRECTION('ref_axis',(1.,0.,0.));
#8001=DIRECTION('',(0.,-1.,0.));
#8002=DIRECTION('center_axis',(0.,1.,0.));
#8003=DIRECTION('ref_axis',(1.,0.,0.));
#8004=DIRECTION('center_axis',(0.,1.,0.));
#8005=DIRECTION('ref_axis',(1.,0.,0.));
#8006=DIRECTION('center_axis',(0.,-1.,0.));
#8007=DIRECTION('ref_axis',(1.,0.,0.));
#8008=DIRECTION('center_axis',(0.,1.,0.));
#8009=DIRECTION('ref_axis',(1.,0.,0.));
#8010=DIRECTION('center_axis',(0.,-1.,0.));
#8011=DIRECTION('ref_axis',(1.,0.,0.));
#8012=DIRECTION('',(0.,-1.,0.));
#8013=DIRECTION('center_axis',(0.,1.,0.));
#8014=DIRECTION('ref_axis',(1.,0.,0.));
#8015=DIRECTION('center_axis',(0.,1.,0.));
#8016=DIRECTION('ref_axis',(1.,0.,0.));
#8017=DIRECTION('',(0.,-1.,0.));
#8018=DIRECTION('center_axis',(0.,1.,0.));
#8019=DIRECTION('ref_axis',(1.,0.,0.));
#8020=DIRECTION('center_axis',(0.,1.,0.));
#8021=DIRECTION('ref_axis',(1.,0.,0.));
#8022=DIRECTION('center_axis',(0.,1.,0.));
#8023=DIRECTION('ref_axis',(1.,0.,0.));
#8024=DIRECTION('axis',(0.,0.,1.));
#8025=DIRECTION('refdir',(1.,0.,0.));
#8026=DIRECTION('center_axis',(0.,0.,1.));
#8027=DIRECTION('ref_axis',(1.,0.,0.));
#8028=DIRECTION('center_axis',(0.,0.,1.));
#8029=DIRECTION('ref_axis',(1.,0.,0.));
#8030=DIRECTION('',(0.,0.,1.));
#8031=DIRECTION('center_axis',(0.,0.,-1.));
#8032=DIRECTION('ref_axis',(1.,0.,0.));
#8033=DIRECTION('center_axis',(0.,0.,1.));
#8034=DIRECTION('ref_axis',(1.,0.,0.));
#8035=DIRECTION('center_axis',(0.,0.,1.));
#8036=DIRECTION('ref_axis',(1.,0.,0.));
#8037=DIRECTION('',(0.,0.,1.));
#8038=DIRECTION('center_axis',(0.,0.,-1.));
#8039=DIRECTION('ref_axis',(1.,0.,0.));
#8040=DIRECTION('center_axis',(0.,1.,0.));
#8041=DIRECTION('ref_axis',(1.,0.,0.));
#8042=DIRECTION('center_axis',(0.,1.,0.));
#8043=DIRECTION('ref_axis',(1.,0.,0.));
#8044=DIRECTION('',(0.,1.,0.));
#8045=DIRECTION('center_axis',(0.,-1.,0.));
#8046=DIRECTION('ref_axis',(1.,0.,0.));
#8047=DIRECTION('center_axis',(0.,1.,0.));
#8048=DIRECTION('ref_axis',(1.,0.,0.));
#8049=DIRECTION('center_axis',(0.,1.,0.));
#8050=DIRECTION('ref_axis',(1.,0.,0.));
#8051=DIRECTION('',(0.,1.,0.));
#8052=DIRECTION('center_axis',(0.,-1.,0.));
#8053=DIRECTION('ref_axis',(1.,0.,0.));
#8054=DIRECTION('center_axis',(0.,1.,0.));
#8055=DIRECTION('ref_axis',(1.,0.,0.));
#8056=DIRECTION('center_axis',(0.,1.,0.));
#8057=DIRECTION('ref_axis',(1.,0.,0.));
#8058=DIRECTION('',(0.,1.,0.));
#8059=DIRECTION('center_axis',(0.,-1.,0.));
#8060=DIRECTION('ref_axis',(1.,0.,0.));
#8061=DIRECTION('center_axis',(0.,1.,0.));
#8062=DIRECTION('ref_axis',(1.,0.,0.));
#8063=DIRECTION('center_axis',(0.,1.,0.));
#8064=DIRECTION('ref_axis',(1.,0.,0.));
#8065=DIRECTION('',(0.,1.,0.));
#8066=DIRECTION('center_axis',(0.,-1.,0.));
#8067=DIRECTION('ref_axis',(1.,0.,0.));
#8068=DIRECTION('center_axis',(0.,1.,0.));
#8069=DIRECTION('ref_axis',(1.,0.,0.));
#8070=DIRECTION('center_axis',(0.,1.,0.));
#8071=DIRECTION('ref_axis',(1.,0.,0.));
#8072=DIRECTION('',(0.,1.,0.));
#8073=DIRECTION('center_axis',(0.,-1.,0.));
#8074=DIRECTION('ref_axis',(1.,0.,0.));
#8075=DIRECTION('center_axis',(0.,0.,1.));
#8076=DIRECTION('ref_axis',(1.,0.,0.));
#8077=DIRECTION('',(0.,1.,0.));
#8078=DIRECTION('',(-1.,0.,0.));
#8079=DIRECTION('',(0.,1.,0.));
#8080=DIRECTION('',(1.,0.,0.));
#8081=DIRECTION('center_axis',(0.,0.,1.));
#8082=DIRECTION('ref_axis',(1.,0.,0.));
#8083=DIRECTION('',(0.,-1.,0.));
#8084=DIRECTION('',(1.,0.,0.));
#8085=DIRECTION('',(0.,1.,0.));
#8086=DIRECTION('',(-1.,0.,0.));
#8087=DIRECTION('center_axis',(-1.,0.,0.));
#8088=DIRECTION('ref_axis',(0.,0.,1.));
#8089=DIRECTION('',(0.,0.,-1.));
#8090=DIRECTION('',(0.,0.,1.));
#8091=DIRECTION('',(0.,1.,0.));
#8092=DIRECTION('center_axis',(1.,0.,0.));
#8093=DIRECTION('ref_axis',(0.,0.,-1.));
#8094=DIRECTION('',(0.,0.,1.));
#8095=DIRECTION('',(0.,1.,0.));
#8096=DIRECTION('',(0.,0.,-1.));
#8097=DIRECTION('center_axis',(0.,-1.,0.));
#8098=DIRECTION('ref_axis',(1.,0.,0.));
#8099=DIRECTION('',(0.,0.,1.));
#8100=DIRECTION('',(1.,0.,0.));
#8101=DIRECTION('',(0.,0.,1.));
#8102=DIRECTION('',(1.,0.,0.));
#8103=DIRECTION('center_axis',(1.,0.,0.));
#8104=DIRECTION('ref_axis',(0.,1.,0.));
#8105=DIRECTION('',(0.,0.,1.));
#8106=DIRECTION('',(0.,1.,0.));
#8107=DIRECTION('center_axis',(0.,1.,0.));
#8108=DIRECTION('ref_axis',(-1.,0.,0.));
#8109=DIRECTION('',(0.,0.,1.));
#8110=DIRECTION('',(-1.,0.,0.));
#8111=DIRECTION('',(-1.,0.,0.));
#8112=DIRECTION('center_axis',(-1.,0.,0.));
#8113=DIRECTION('ref_axis',(0.,-1.,0.));
#8114=DIRECTION('',(0.,-1.,0.));
#8115=DIRECTION('center_axis',(0.,0.,1.));
#8116=DIRECTION('ref_axis',(1.,0.,0.));
#8117=DIRECTION('center_axis',(0.,0.,1.));
#8118=DIRECTION('ref_axis',(1.,0.,0.));
#8119=DIRECTION('axis',(0.,0.,1.));
#8120=DIRECTION('refdir',(1.,0.,0.));
#8121=DIRECTION('center_axis',(0.,1.,0.));
#8122=DIRECTION('ref_axis',(1.,0.,0.));
#8123=DIRECTION('center_axis',(0.,1.,0.));
#8124=DIRECTION('ref_axis',(1.,0.,0.));
#8125=DIRECTION('',(0.,1.,0.));
#8126=DIRECTION('center_axis',(0.,-1.,0.));
#8127=DIRECTION('ref_axis',(1.,0.,0.));
#8128=DIRECTION('center_axis',(0.,1.,0.));
#8129=DIRECTION('ref_axis',(1.,0.,0.));
#8130=DIRECTION('center_axis',(0.,1.,0.));
#8131=DIRECTION('ref_axis',(1.,0.,0.));
#8132=DIRECTION('',(0.,1.,0.));
#8133=DIRECTION('center_axis',(0.,-1.,0.));
#8134=DIRECTION('ref_axis',(1.,0.,0.));
#8135=DIRECTION('center_axis',(0.,1.,0.));
#8136=DIRECTION('ref_axis',(1.,0.,0.));
#8137=DIRECTION('center_axis',(0.,1.,0.));
#8138=DIRECTION('ref_axis',(1.,0.,0.));
#8139=DIRECTION('',(0.,1.,0.));
#8140=DIRECTION('center_axis',(0.,-1.,0.));
#8141=DIRECTION('ref_axis',(1.,0.,0.));
#8142=DIRECTION('center_axis',(0.,1.,0.));
#8143=DIRECTION('ref_axis',(1.,0.,0.));
#8144=DIRECTION('center_axis',(0.,1.,0.));
#8145=DIRECTION('ref_axis',(1.,0.,0.));
#8146=DIRECTION('',(0.,1.,0.));
#8147=DIRECTION('center_axis',(0.,-1.,0.));
#8148=DIRECTION('ref_axis',(1.,0.,0.));
#8149=DIRECTION('center_axis',(0.,1.,0.));
#8150=DIRECTION('ref_axis',(1.,0.,0.));
#8151=DIRECTION('center_axis',(0.,1.,0.));
#8152=DIRECTION('ref_axis',(1.,0.,0.));
#8153=DIRECTION('',(0.,-1.,0.));
#8154=DIRECTION('center_axis',(0.,-1.,0.));
#8155=DIRECTION('ref_axis',(1.,0.,0.));
#8156=DIRECTION('center_axis',(0.,1.,0.));
#8157=DIRECTION('ref_axis',(1.,0.,0.));
#8158=DIRECTION('center_axis',(0.,-1.,0.));
#8159=DIRECTION('ref_axis',(1.,0.,0.));
#8160=DIRECTION('center_axis',(0.,1.,0.));
#8161=DIRECTION('ref_axis',(1.,0.,0.));
#8162=DIRECTION('',(0.,-1.,0.));
#8163=DIRECTION('center_axis',(0.,-1.,0.));
#8164=DIRECTION('ref_axis',(1.,0.,0.));
#8165=DIRECTION('center_axis',(0.,1.,0.));
#8166=DIRECTION('ref_axis',(1.,0.,0.));
#8167=DIRECTION('center_axis',(0.,1.,0.));
#8168=DIRECTION('ref_axis',(1.,0.,0.));
#8169=DIRECTION('',(0.,-1.,0.));
#8170=DIRECTION('center_axis',(0.,1.,0.));
#8171=DIRECTION('ref_axis',(1.,0.,0.));
#8172=DIRECTION('center_axis',(0.,1.,0.));
#8173=DIRECTION('ref_axis',(1.,0.,0.));
#8174=DIRECTION('center_axis',(0.,1.,0.));
#8175=DIRECTION('ref_axis',(1.,0.,0.));
#8176=DIRECTION('axis',(0.,0.,1.));
#8177=DIRECTION('refdir',(1.,0.,0.));
#8178=DIRECTION('center_axis',(0.,1.,0.));
#8179=DIRECTION('ref_axis',(1.,0.,0.));
#8180=DIRECTION('center_axis',(0.,1.,0.));
#8181=DIRECTION('ref_axis',(1.,0.,0.));
#8182=DIRECTION('',(0.,1.,0.));
#8183=DIRECTION('center_axis',(0.,-1.,0.));
#8184=DIRECTION('ref_axis',(1.,0.,0.));
#8185=DIRECTION('center_axis',(0.,1.,0.));
#8186=DIRECTION('ref_axis',(1.,0.,0.));
#8187=DIRECTION('center_axis',(0.,1.,0.));
#8188=DIRECTION('ref_axis',(1.,0.,0.));
#8189=DIRECTION('',(0.,1.,0.));
#8190=DIRECTION('center_axis',(0.,-1.,0.));
#8191=DIRECTION('ref_axis',(1.,0.,0.));
#8192=DIRECTION('center_axis',(0.,1.,0.));
#8193=DIRECTION('ref_axis',(1.,0.,0.));
#8194=DIRECTION('center_axis',(0.,1.,0.));
#8195=DIRECTION('ref_axis',(1.,0.,0.));
#8196=DIRECTION('',(0.,1.,0.));
#8197=DIRECTION('center_axis',(0.,-1.,0.));
#8198=DIRECTION('ref_axis',(1.,0.,0.));
#8199=DIRECTION('center_axis',(0.,1.,0.));
#8200=DIRECTION('ref_axis',(1.,0.,0.));
#8201=DIRECTION('center_axis',(0.,1.,0.));
#8202=DIRECTION('ref_axis',(1.,0.,0.));
#8203=DIRECTION('',(0.,1.,0.));
#8204=DIRECTION('center_axis',(0.,-1.,0.));
#8205=DIRECTION('ref_axis',(1.,0.,0.));
#8206=DIRECTION('center_axis',(0.,1.,0.));
#8207=DIRECTION('ref_axis',(1.,0.,0.));
#8208=DIRECTION('center_axis',(0.,1.,0.));
#8209=DIRECTION('ref_axis',(1.,0.,0.));
#8210=DIRECTION('',(0.,-1.,0.));
#8211=DIRECTION('center_axis',(0.,1.,0.));
#8212=DIRECTION('ref_axis',(1.,0.,0.));
#8213=DIRECTION('center_axis',(0.,1.,0.));
#8214=DIRECTION('ref_axis',(1.,0.,0.));
#8215=DIRECTION('center_axis',(0.,-1.,0.));
#8216=DIRECTION('ref_axis',(1.,0.,0.));
#8217=DIRECTION('center_axis',(0.,1.,0.));
#8218=DIRECTION('ref_axis',(1.,0.,0.));
#8219=DIRECTION('center_axis',(0.,-1.,0.));
#8220=DIRECTION('ref_axis',(1.,0.,0.));
#8221=DIRECTION('',(0.,-1.,0.));
#8222=DIRECTION('center_axis',(0.,1.,0.));
#8223=DIRECTION('ref_axis',(1.,0.,0.));
#8224=DIRECTION('center_axis',(0.,1.,0.));
#8225=DIRECTION('ref_axis',(1.,0.,0.));
#8226=DIRECTION('',(0.,-1.,0.));
#8227=DIRECTION('center_axis',(0.,1.,0.));
#8228=DIRECTION('ref_axis',(1.,0.,0.));
#8229=DIRECTION('center_axis',(0.,1.,0.));
#8230=DIRECTION('ref_axis',(1.,0.,0.));
#8231=DIRECTION('center_axis',(0.,1.,0.));
#8232=DIRECTION('ref_axis',(1.,0.,0.));
#8233=DIRECTION('axis',(0.,0.,1.));
#8234=DIRECTION('refdir',(1.,0.,0.));
#8235=DIRECTION('center_axis',(0.,0.,1.));
#8236=DIRECTION('ref_axis',(1.,0.,0.));
#8237=DIRECTION('center_axis',(0.,0.,1.));
#8238=DIRECTION('ref_axis',(1.,0.,0.));
#8239=DIRECTION('',(0.,0.,1.));
#8240=DIRECTION('center_axis',(0.,0.,-1.));
#8241=DIRECTION('ref_axis',(1.,0.,0.));
#8242=DIRECTION('center_axis',(0.,0.,1.));
#8243=DIRECTION('ref_axis',(1.,0.,0.));
#8244=DIRECTION('center_axis',(0.,0.,1.));
#8245=DIRECTION('ref_axis',(1.,0.,0.));
#8246=DIRECTION('center_axis',(0.,0.,1.));
#8247=DIRECTION('ref_axis',(1.,0.,0.));
#8248=DIRECTION('',(0.,0.,1.));
#8249=DIRECTION('center_axis',(0.,0.,-1.));
#8250=DIRECTION('ref_axis',(1.,0.,0.));
#8251=DIRECTION('center_axis',(0.,0.,1.));
#8252=DIRECTION('ref_axis',(1.,0.,0.));
#8253=DIRECTION('center_axis',(0.,0.,1.));
#8254=DIRECTION('ref_axis',(1.,0.,0.));
#8255=DIRECTION('center_axis',(0.,0.,1.));
#8256=DIRECTION('ref_axis',(1.,0.,0.));
#8257=DIRECTION('',(0.,0.,1.));
#8258=DIRECTION('center_axis',(0.,0.,-1.));
#8259=DIRECTION('ref_axis',(1.,0.,0.));
#8260=DIRECTION('center_axis',(0.,0.,1.));
#8261=DIRECTION('ref_axis',(1.,0.,0.));
#8262=DIRECTION('center_axis',(0.,0.,1.));
#8263=DIRECTION('ref_axis',(1.,0.,0.));
#8264=DIRECTION('center_axis',(0.,0.,1.));
#8265=DIRECTION('ref_axis',(1.,0.,0.));
#8266=DIRECTION('',(0.,0.,1.));
#8267=DIRECTION('center_axis',(0.,0.,-1.));
#8268=DIRECTION('ref_axis',(1.,0.,0.));
#8269=DIRECTION('center_axis',(0.,0.,1.));
#8270=DIRECTION('ref_axis',(1.,0.,0.));
#8271=DIRECTION('center_axis',(0.,0.,1.));
#8272=DIRECTION('ref_axis',(1.,0.,0.));
#8273=DIRECTION('center_axis',(0.,0.,1.));
#8274=DIRECTION('ref_axis',(1.,0.,0.));
#8275=DIRECTION('',(0.,0.,1.));
#8276=DIRECTION('center_axis',(0.,0.,-1.));
#8277=DIRECTION('ref_axis',(1.,0.,0.));
#8278=DIRECTION('center_axis',(0.,0.,1.));
#8279=DIRECTION('ref_axis',(1.,0.,0.));
#8280=DIRECTION('center_axis',(0.,0.,1.));
#8281=DIRECTION('ref_axis',(1.,0.,0.));
#8282=DIRECTION('center_axis',(0.,0.,1.));
#8283=DIRECTION('ref_axis',(1.,0.,0.));
#8284=DIRECTION('center_axis',(0.,0.,1.));
#8285=DIRECTION('ref_axis',(1.,0.,0.));
#8286=DIRECTION('',(0.,0.,1.));
#8287=DIRECTION('center_axis',(0.,0.,1.));
#8288=DIRECTION('ref_axis',(1.,0.,0.));
#8289=DIRECTION('center_axis',(0.,0.,1.));
#8290=DIRECTION('ref_axis',(1.,0.,0.));
#8291=DIRECTION('',(0.,0.,1.));
#8292=DIRECTION('center_axis',(0.,0.,-1.));
#8293=DIRECTION('ref_axis',(1.,0.,0.));
#8294=DIRECTION('center_axis',(0.,0.,1.));
#8295=DIRECTION('ref_axis',(1.,0.,0.));
#8296=DIRECTION('center_axis',(0.,0.,1.));
#8297=DIRECTION('ref_axis',(1.,0.,0.));
#8298=DIRECTION('center_axis',(0.,0.,1.));
#8299=DIRECTION('ref_axis',(1.,0.,0.));
#8300=DIRECTION('center_axis',(0.,0.,1.));
#8301=DIRECTION('ref_axis',(1.,0.,0.));
#8302=DIRECTION('',(0.,0.,1.));
#8303=DIRECTION('center_axis',(0.,0.,1.));
#8304=DIRECTION('ref_axis',(1.,0.,0.));
#8305=DIRECTION('center_axis',(0.,0.,1.));
#8306=DIRECTION('ref_axis',(1.,0.,0.));
#8307=DIRECTION('',(0.,0.,1.));
#8308=DIRECTION('center_axis',(0.,0.,-1.));
#8309=DIRECTION('ref_axis',(1.,0.,0.));
#8310=DIRECTION('center_axis',(0.,0.,1.));
#8311=DIRECTION('ref_axis',(1.,0.,0.));
#8312=DIRECTION('center_axis',(0.,0.,1.));
#8313=DIRECTION('ref_axis',(1.,0.,0.));
#8314=DIRECTION('center_axis',(0.,0.,1.));
#8315=DIRECTION('ref_axis',(1.,0.,0.));
#8316=DIRECTION('center_axis',(0.,0.,1.));
#8317=DIRECTION('ref_axis',(1.,0.,0.));
#8318=DIRECTION('',(0.,0.,1.));
#8319=DIRECTION('center_axis',(0.,0.,-1.));
#8320=DIRECTION('ref_axis',(-1.,0.,0.));
#8321=DIRECTION('',(1.,0.,0.));
#8322=DIRECTION('',(0.,1.,0.));
#8323=DIRECTION('',(-1.,0.,0.));
#8324=DIRECTION('',(0.,1.,0.));
#8325=DIRECTION('',(1.,0.,0.));
#8326=DIRECTION('',(0.,1.,0.));
#8327=DIRECTION('',(-1.,0.,0.));
#8328=DIRECTION('',(0.,1.,0.));
#8329=DIRECTION('',(1.,0.,0.));
#8330=DIRECTION('',(0.,1.,0.));
#8331=DIRECTION('',(-1.,0.,0.));
#8332=DIRECTION('',(0.,-1.,0.));
#8333=DIRECTION('center_axis',(0.,1.,0.));
#8334=DIRECTION('ref_axis',(0.,0.,1.));
#8335=DIRECTION('',(1.,0.,0.));
#8336=DIRECTION('',(0.,0.,-1.));
#8337=DIRECTION('',(0.,0.,1.));
#8338=DIRECTION('center_axis',(0.,1.,0.));
#8339=DIRECTION('ref_axis',(1.,0.,0.));
#8340=DIRECTION('',(-1.,0.,0.));
#8341=DIRECTION('',(0.,0.,-1.));
#8342=DIRECTION('',(0.,0.,1.));
#8343=DIRECTION('center_axis',(-1.,0.,0.));
#8344=DIRECTION('ref_axis',(0.,0.,1.));
#8345=DIRECTION('',(0.,0.,1.));
#8346=DIRECTION('',(0.,1.,0.));
#8347=DIRECTION('',(0.,0.,-1.));
#8348=DIRECTION('center_axis',(0.,1.,0.));
#8349=DIRECTION('ref_axis',(0.,0.,1.));
#8350=DIRECTION('',(0.,0.,-1.));
#8351=DIRECTION('',(-1.,0.,0.));
#8352=DIRECTION('center_axis',(0.,0.,-1.));
#8353=DIRECTION('ref_axis',(-1.,0.,0.));
#8354=DIRECTION('',(1.,0.,0.));
#8355=DIRECTION('',(0.,1.,0.));
#8356=DIRECTION('center_axis',(1.,0.,0.));
#8357=DIRECTION('ref_axis',(0.,0.,-1.));
#8358=DIRECTION('',(0.,0.,1.));
#8359=DIRECTION('',(0.,1.,0.));
#8360=DIRECTION('center_axis',(0.,1.,0.));
#8361=DIRECTION('ref_axis',(1.,0.,0.));
#8362=DIRECTION('center_axis',(1.,0.,0.));
#8363=DIRECTION('ref_axis',(0.,1.,0.));
#8364=DIRECTION('',(0.,0.,1.));
#8365=DIRECTION('',(0.,1.,0.));
#8366=DIRECTION('',(0.,0.,1.));
#8367=DIRECTION('center_axis',(0.,-1.,0.));
#8368=DIRECTION('ref_axis',(1.,0.,0.));
#8369=DIRECTION('',(0.,0.,1.));
#8370=DIRECTION('',(1.,0.,0.));
#8371=DIRECTION('center_axis',(0.,1.,0.));
#8372=DIRECTION('ref_axis',(-1.,0.,0.));
#8373=DIRECTION('',(-1.,0.,0.));
#8374=DIRECTION('',(0.,0.,1.));
#8375=DIRECTION('center_axis',(-1.,0.,0.));
#8376=DIRECTION('ref_axis',(0.,-1.,0.));
#8377=DIRECTION('',(0.,-1.,0.));
#8378=DIRECTION('',(0.,1.,0.));
#8379=DIRECTION('center_axis',(0.,0.,1.));
#8380=DIRECTION('ref_axis',(1.,0.,0.));
#8381=DIRECTION('center_axis',(0.,0.,1.));
#8382=DIRECTION('ref_axis',(1.,0.,0.));
#8383=DIRECTION('axis',(0.,0.,1.));
#8384=DIRECTION('refdir',(1.,0.,0.));
#8385=DIRECTION('center_axis',(0.,0.,1.));
#8386=DIRECTION('ref_axis',(1.,0.,0.));
#8387=DIRECTION('center_axis',(0.,0.,-1.));
#8388=DIRECTION('ref_axis',(1.,0.,0.));
#8389=DIRECTION('',(0.,0.,-1.));
#8390=DIRECTION('center_axis',(0.,0.,-1.));
#8391=DIRECTION('ref_axis',(1.,0.,0.));
#8392=DIRECTION('center_axis',(0.,0.,1.));
#8393=DIRECTION('ref_axis',(1.,0.,0.));
#8394=DIRECTION('center_axis',(0.,0.,1.));
#8395=DIRECTION('ref_axis',(1.,0.,0.));
#8396=DIRECTION('',(0.,0.,-1.));
#8397=DIRECTION('center_axis',(0.,0.,1.));
#8398=DIRECTION('ref_axis',(1.,0.,0.));
#8399=DIRECTION('center_axis',(0.,0.,1.));
#8400=DIRECTION('ref_axis',(1.,0.,0.));
#8401=DIRECTION('center_axis',(0.,0.,1.));
#8402=DIRECTION('ref_axis',(1.,0.,0.));
#8403=DIRECTION('axis',(0.,0.,1.));
#8404=DIRECTION('refdir',(1.,0.,0.));
#8405=DIRECTION('center_axis',(0.,0.,1.));
#8406=DIRECTION('ref_axis',(1.,0.,0.));
#8407=DIRECTION('center_axis',(0.,0.,1.));
#8408=DIRECTION('ref_axis',(1.,0.,0.));
#8409=DIRECTION('',(0.,0.,1.));
#8410=DIRECTION('center_axis',(0.,0.,-1.));
#8411=DIRECTION('ref_axis',(1.,0.,0.));
#8412=DIRECTION('center_axis',(0.,0.,1.));
#8413=DIRECTION('ref_axis',(1.,0.,0.));
#8414=DIRECTION('center_axis',(0.,0.,1.));
#8415=DIRECTION('ref_axis',(1.,0.,0.));
#8416=DIRECTION('',(0.,0.,1.));
#8417=DIRECTION('center_axis',(0.,0.,-1.));
#8418=DIRECTION('ref_axis',(1.,0.,0.));
#8419=DIRECTION('center_axis',(0.,0.,1.));
#8420=DIRECTION('ref_axis',(1.,0.,0.));
#8421=DIRECTION('center_axis',(0.,0.,1.));
#8422=DIRECTION('ref_axis',(1.,0.,0.));
#8423=DIRECTION('',(0.,0.,1.));
#8424=DIRECTION('center_axis',(0.,0.,-1.));
#8425=DIRECTION('ref_axis',(1.,0.,0.));
#8426=DIRECTION('center_axis',(0.,0.,1.));
#8427=DIRECTION('ref_axis',(1.,0.,0.));
#8428=DIRECTION('center_axis',(0.,0.,1.));
#8429=DIRECTION('ref_axis',(1.,0.,0.));
#8430=DIRECTION('',(0.,0.,1.));
#8431=DIRECTION('center_axis',(0.,0.,-1.));
#8432=DIRECTION('ref_axis',(1.,0.,0.));
#8433=DIRECTION('center_axis',(0.,0.,1.));
#8434=DIRECTION('ref_axis',(1.,0.,0.));
#8435=DIRECTION('center_axis',(0.,0.,1.));
#8436=DIRECTION('ref_axis',(1.,0.,0.));
#8437=DIRECTION('',(0.,0.,-1.));
#8438=DIRECTION('center_axis',(0.,0.,1.));
#8439=DIRECTION('ref_axis',(1.,0.,0.));
#8440=DIRECTION('center_axis',(0.,0.,1.));
#8441=DIRECTION('ref_axis',(1.,0.,0.));
#8442=DIRECTION('center_axis',(0.,0.,-1.));
#8443=DIRECTION('ref_axis',(1.,0.,0.));
#8444=DIRECTION('center_axis',(0.,0.,1.));
#8445=DIRECTION('ref_axis',(1.,0.,0.));
#8446=DIRECTION('center_axis',(0.,0.,-1.));
#8447=DIRECTION('ref_axis',(1.,0.,0.));
#8448=DIRECTION('',(0.,0.,-1.));
#8449=DIRECTION('center_axis',(0.,0.,1.));
#8450=DIRECTION('ref_axis',(1.,0.,0.));
#8451=DIRECTION('center_axis',(0.,0.,1.));
#8452=DIRECTION('ref_axis',(1.,0.,0.));
#8453=DIRECTION('',(0.,0.,-1.));
#8454=DIRECTION('center_axis',(0.,0.,1.));
#8455=DIRECTION('ref_axis',(1.,0.,0.));
#8456=DIRECTION('center_axis',(0.,0.,1.));
#8457=DIRECTION('ref_axis',(1.,0.,0.));
#8458=DIRECTION('center_axis',(0.,0.,1.));
#8459=DIRECTION('ref_axis',(1.,0.,0.));
#8460=DIRECTION('axis',(0.,0.,1.));
#8461=DIRECTION('refdir',(1.,0.,0.));
#8462=DIRECTION('center_axis',(-0.000134463754131944,0.998830887797922,
0.0483408678067963));
#8463=DIRECTION('ref_axis',(6.50770273904549E-6,-0.0483408673687592,0.998830896848754));
#8464=DIRECTION('center_axis',(0.000134463742439319,0.998830887795465,0.0483408678575998));
#8465=DIRECTION('ref_axis',(-0.0950425701692232,0.0481348041224881,-0.994308780252753));
#8466=DIRECTION('center_axis',(0.000134463742439319,0.998830887795465,0.0483408678575998));
#8467=DIRECTION('ref_axis',(-0.0950425701692232,0.0481348041224881,-0.994308780252753));
#8468=DIRECTION('center_axis',(-0.000134463754131944,0.998830887797922,
0.0483408678067963));
#8469=DIRECTION('ref_axis',(6.50770273904549E-6,-0.0483408673687592,0.998830896848754));
#8470=DIRECTION('axis',(0.,0.,1.));
#8471=DIRECTION('refdir',(1.,0.,0.));
#8472=DIRECTION('axis',(0.,0.,1.));
#8473=DIRECTION('refdir',(1.,0.,0.));
#8474=DIRECTION('center_axis',(0.,-1.,0.));
#8475=DIRECTION('ref_axis',(0.,0.,-1.));
#8476=DIRECTION('center_axis',(0.,-1.,0.));
#8477=DIRECTION('ref_axis',(1.,0.,0.));
#8478=DIRECTION('center_axis',(0.,-1.,0.));
#8479=DIRECTION('ref_axis',(1.,0.,0.));
#8480=DIRECTION('center_axis',(1.,0.,1.22464679914735E-16));
#8481=DIRECTION('ref_axis',(-1.22464679914735E-16,0.,1.));
#8482=DIRECTION('center_axis',(0.,1.,0.));
#8483=DIRECTION('ref_axis',(1.,0.,0.));
#8484=DIRECTION('center_axis',(0.,1.,0.));
#8485=DIRECTION('ref_axis',(1.,0.,0.));
#8486=DIRECTION('center_axis',(0.,-1.,0.));
#8487=DIRECTION('ref_axis',(1.,0.,0.));
#8488=DIRECTION('',(0.,1.,0.));
#8489=DIRECTION('center_axis',(0.,-1.,0.));
#8490=DIRECTION('ref_axis',(1.,0.,0.));
#8491=DIRECTION('center_axis',(0.,-1.,0.));
#8492=DIRECTION('ref_axis',(1.,0.,0.));
#8493=DIRECTION('center_axis',(0.,-1.,0.));
#8494=DIRECTION('ref_axis',(1.,0.,0.));
#8495=DIRECTION('',(0.,1.,0.));
#8496=DIRECTION('center_axis',(0.,-1.,0.));
#8497=DIRECTION('ref_axis',(1.,0.,0.));
#8498=DIRECTION('center_axis',(0.,1.,0.));
#8499=DIRECTION('ref_axis',(1.,0.,0.));
#8500=DIRECTION('',(-0.707106781186548,0.707106781186547,-8.65956056235493E-17));
#8501=DIRECTION('center_axis',(0.,-1.,0.));
#8502=DIRECTION('ref_axis',(1.,0.,0.));
#8503=DIRECTION('center_axis',(0.,1.,0.));
#8504=DIRECTION('ref_axis',(0.,0.,1.));
#8505=DIRECTION('center_axis',(0.,-1.,0.));
#8506=DIRECTION('ref_axis',(1.,0.,0.));
#8507=DIRECTION('center_axis',(0.,-1.,0.));
#8508=DIRECTION('ref_axis',(1.,0.,0.));
#8509=DIRECTION('',(0.,1.,0.));
#8510=DIRECTION('center_axis',(0.,-1.,0.));
#8511=DIRECTION('ref_axis',(0.,0.,-1.));
#8512=DIRECTION('center_axis',(0.,-1.,0.));
#8513=DIRECTION('ref_axis',(1.,0.,0.));
#8514=DIRECTION('center_axis',(0.,-1.,0.));
#8515=DIRECTION('ref_axis',(1.,0.,0.));
#8516=DIRECTION('',(0.707106781186548,0.707106781186547,8.65956056235493E-17));
#8517=DIRECTION('axis',(0.,0.,1.));
#8518=DIRECTION('refdir',(1.,0.,0.));
#8519=DIRECTION('center_axis',(0.,-1.,0.));
#8520=DIRECTION('ref_axis',(0.,0.,-1.));
#8521=DIRECTION('center_axis',(0.,-1.,0.));
#8522=DIRECTION('ref_axis',(1.,0.,0.));
#8523=DIRECTION('center_axis',(0.,-1.,0.));
#8524=DIRECTION('ref_axis',(1.,0.,0.));
#8525=DIRECTION('center_axis',(1.,0.,1.22464679914735E-16));
#8526=DIRECTION('ref_axis',(-1.22464679914735E-16,0.,1.));
#8527=DIRECTION('center_axis',(0.,1.,0.));
#8528=DIRECTION('ref_axis',(1.,0.,0.));
#8529=DIRECTION('center_axis',(0.,1.,0.));
#8530=DIRECTION('ref_axis',(1.,0.,0.));
#8531=DIRECTION('center_axis',(0.,-1.,0.));
#8532=DIRECTION('ref_axis',(1.,0.,0.));
#8533=DIRECTION('center_axis',(0.,-1.,0.));
#8534=DIRECTION('ref_axis',(1.,0.,0.));
#8535=DIRECTION('',(0.,1.,0.));
#8536=DIRECTION('center_axis',(0.,1.,0.));
#8537=DIRECTION('ref_axis',(0.,0.,1.));
#8538=DIRECTION('center_axis',(0.,-1.,0.));
#8539=DIRECTION('ref_axis',(1.,0.,0.));
#8540=DIRECTION('center_axis',(0.,-1.,0.));
#8541=DIRECTION('ref_axis',(1.,0.,0.));
#8542=DIRECTION('center_axis',(0.,-1.,0.));
#8543=DIRECTION('ref_axis',(1.,0.,0.));
#8544=DIRECTION('center_axis',(0.,-1.,0.));
#8545=DIRECTION('ref_axis',(1.,0.,0.));
#8546=DIRECTION('',(0.707106781186548,0.707106781186547,8.65956056235494E-17));
#8547=DIRECTION('center_axis',(0.,-1.,0.));
#8548=DIRECTION('ref_axis',(1.,0.,0.));
#8549=DIRECTION('center_axis',(0.,-1.,0.));
#8550=DIRECTION('ref_axis',(1.,0.,0.));
#8551=DIRECTION('',(0.,1.,0.));
#8552=DIRECTION('center_axis',(0.,1.,0.));
#8553=DIRECTION('ref_axis',(1.,0.,0.));
#8554=DIRECTION('center_axis',(0.,-1.,0.));
#8555=DIRECTION('ref_axis',(1.,0.,0.));
#8556=DIRECTION('',(-0.707106781186548,0.707106781186547,-8.65956056235494E-17));
#8557=DIRECTION('center_axis',(0.,-1.,0.));
#8558=DIRECTION('ref_axis',(0.,0.,-1.));
#8559=DIRECTION('center_axis',(0.,-1.,0.));
#8560=DIRECTION('ref_axis',(1.,0.,0.));
#8561=DIRECTION('',(0.,1.,0.));
#8562=DIRECTION('axis',(0.,0.,1.));
#8563=DIRECTION('refdir',(1.,0.,0.));
#8564=DIRECTION('center_axis',(0.,0.,1.));
#8565=DIRECTION('ref_axis',(1.,0.,0.));
#8566=DIRECTION('center_axis',(1.22464679914735E-16,-1.,0.));
#8567=DIRECTION('ref_axis',(-1.,-1.22464679914735E-16,0.));
#8568=DIRECTION('center_axis',(0.78183148246803,0.,0.623489801858733));
#8569=DIRECTION('ref_axis',(0.623489801858734,0.,-0.78183148246803));
#8570=DIRECTION('center_axis',(7.63554790147315E-17,-1.,-9.57467422477103E-17));
#8571=DIRECTION('ref_axis',(-0.623489801858734,-1.22464679914735E-16,0.78183148246803));
#8572=DIRECTION('center_axis',(0.974927912181824,0.,-0.222520933956314));
#8573=DIRECTION('ref_axis',(-0.222520933956314,0.,-0.974927912181824));
#8574=DIRECTION('center_axis',(-2.7250954951288E-17,-1.,-1.19394234705288E-16));
#8575=DIRECTION('ref_axis',(0.222520933956314,-1.22464679914735E-16,0.974927912181824));
#8576=DIRECTION('center_axis',(0.433883739117558,0.,-0.900968867902419));
#8577=DIRECTION('ref_axis',(-0.900968867902419,0.,-0.433883739117558));
#8578=DIRECTION('center_axis',(-1.10336864020811E-16,-1.,-5.31354332312403E-17));
#8579=DIRECTION('ref_axis',(0.900968867902419,-1.22464679914735E-16,0.433883739117558));
#8580=DIRECTION('center_axis',(-0.433883739117558,0.,-0.900968867902419));
#8581=DIRECTION('ref_axis',(-0.900968867902419,0.,0.433883739117558));
#8582=DIRECTION('center_axis',(-1.10336864020811E-16,-1.,5.31354332312403E-17));
#8583=DIRECTION('ref_axis',(0.900968867902419,-1.22464679914735E-16,-0.433883739117558));
#8584=DIRECTION('center_axis',(-0.974927912181824,0.,-0.222520933956314));
#8585=DIRECTION('ref_axis',(-0.222520933956315,0.,0.974927912181824));
#8586=DIRECTION('center_axis',(-2.7250954951288E-17,-1.,1.19394234705288E-16));
#8587=DIRECTION('ref_axis',(0.222520933956315,-1.22464679914735E-16,-0.974927912181824));
#8588=DIRECTION('center_axis',(-0.78183148246803,0.,0.623489801858734));
#8589=DIRECTION('ref_axis',(0.623489801858733,0.,0.78183148246803));
#8590=DIRECTION('center_axis',(7.63554790147315E-17,-1.,9.57467422477103E-17));
#8591=DIRECTION('ref_axis',(-0.623489801858733,-1.22464679914735E-16,-0.78183148246803));
#8592=DIRECTION('axis',(0.,0.,1.));
#8593=DIRECTION('refdir',(1.,0.,0.));
#8594=DIRECTION('center_axis',(0.,0.,1.));
#8595=DIRECTION('ref_axis',(1.,0.,0.));
#8596=DIRECTION('center_axis',(0.,-1.,0.));
#8597=DIRECTION('ref_axis',(0.,0.,-1.));
#8598=DIRECTION('center_axis',(0.,-1.,0.));
#8599=DIRECTION('ref_axis',(0.,0.,-1.));
#8600=DIRECTION('center_axis',(0.,1.,0.));
#8601=DIRECTION('ref_axis',(1.,0.,0.));
#8602=DIRECTION('center_axis',(0.,1.,0.));
#8603=DIRECTION('ref_axis',(1.,0.,0.));
#8604=DIRECTION('center_axis',(0.,1.,0.));
#8605=DIRECTION('ref_axis',(1.,0.,0.));
#8606=DIRECTION('center_axis',(0.,1.,0.));
#8607=DIRECTION('ref_axis',(1.,0.,0.));
#8608=DIRECTION('',(0.,-1.,0.));
#8609=DIRECTION('center_axis',(0.,-1.,0.));
#8610=DIRECTION('ref_axis',(1.,0.,0.));
#8611=DIRECTION('center_axis',(0.,1.,0.));
#8612=DIRECTION('ref_axis',(1.,0.,0.));
#8613=DIRECTION('center_axis',(0.,1.,0.));
#8614=DIRECTION('ref_axis',(1.,0.,0.));
#8615=DIRECTION('center_axis',(0.,1.,0.));
#8616=DIRECTION('ref_axis',(1.,0.,0.));
#8617=DIRECTION('center_axis',(0.,1.,0.));
#8618=DIRECTION('ref_axis',(1.,0.,0.));
#8619=DIRECTION('center_axis',(0.,1.,0.));
#8620=DIRECTION('ref_axis',(1.,0.,0.));
#8621=DIRECTION('center_axis',(0.,1.,0.));
#8622=DIRECTION('ref_axis',(1.,0.,0.));
#8623=DIRECTION('center_axis',(0.,-1.,0.));
#8624=DIRECTION('ref_axis',(1.,0.,0.));
#8625=DIRECTION('center_axis',(0.,-1.,0.));
#8626=DIRECTION('ref_axis',(0.,0.,-1.));
#8627=DIRECTION('center_axis',(8.96625347776458E-17,0.,1.));
#8628=DIRECTION('ref_axis',(1.,0.,0.));
#8629=DIRECTION('center_axis',(0.,-1.,0.));
#8630=DIRECTION('ref_axis',(0.,0.,-1.));
#8631=DIRECTION('center_axis',(0.,1.,0.));
#8632=DIRECTION('ref_axis',(1.,0.,0.));
#8633=DIRECTION('center_axis',(0.,-1.,0.));
#8634=DIRECTION('ref_axis',(1.,0.,0.));
#8635=DIRECTION('center_axis',(0.,-1.,0.));
#8636=DIRECTION('ref_axis',(0.,0.,-1.));
#8637=DIRECTION('center_axis',(0.,0.,1.));
#8638=DIRECTION('ref_axis',(1.,0.,0.));
#8639=DIRECTION('center_axis',(0.,-1.,0.));
#8640=DIRECTION('ref_axis',(0.,0.,-1.));
#8641=DIRECTION('center_axis',(0.,1.,0.));
#8642=DIRECTION('ref_axis',(1.,0.,0.));
#8643=DIRECTION('center_axis',(0.,-1.,0.));
#8644=DIRECTION('ref_axis',(1.,0.,0.));
#8645=DIRECTION('center_axis',(0.,-1.,0.));
#8646=DIRECTION('ref_axis',(1.,0.,0.));
#8647=DIRECTION('center_axis',(0.,-1.,0.));
#8648=DIRECTION('ref_axis',(0.,0.,-1.));
#8649=DIRECTION('center_axis',(0.,0.,1.));
#8650=DIRECTION('ref_axis',(1.,0.,0.));
#8651=DIRECTION('center_axis',(0.,-1.,0.));
#8652=DIRECTION('ref_axis',(0.,0.,-1.));
#8653=DIRECTION('center_axis',(0.,1.,0.));
#8654=DIRECTION('ref_axis',(1.,0.,0.));
#8655=DIRECTION('center_axis',(0.,-1.,0.));
#8656=DIRECTION('ref_axis',(1.,0.,0.));
#8657=DIRECTION('center_axis',(0.,-1.,0.));
#8658=DIRECTION('ref_axis',(0.,0.,-1.));
#8659=DIRECTION('center_axis',(8.96625347776458E-17,0.,1.));
#8660=DIRECTION('ref_axis',(1.,0.,0.));
#8661=DIRECTION('center_axis',(0.,-1.,0.));
#8662=DIRECTION('ref_axis',(0.,0.,-1.));
#8663=DIRECTION('center_axis',(0.,1.,0.));
#8664=DIRECTION('ref_axis',(1.,0.,0.));
#8665=DIRECTION('center_axis',(0.,-1.,0.));
#8666=DIRECTION('ref_axis',(1.,0.,0.));
#8667=DIRECTION('center_axis',(0.,-1.,0.));
#8668=DIRECTION('ref_axis',(0.,0.,-1.));
#8669=DIRECTION('center_axis',(0.,0.,1.));
#8670=DIRECTION('ref_axis',(1.,0.,0.));
#8671=DIRECTION('center_axis',(0.,-1.,0.));
#8672=DIRECTION('ref_axis',(0.,0.,-1.));
#8673=DIRECTION('center_axis',(0.,1.,0.));
#8674=DIRECTION('ref_axis',(1.,0.,0.));
#8675=DIRECTION('center_axis',(0.,1.,0.));
#8676=DIRECTION('ref_axis',(1.,0.,0.));
#8677=DIRECTION('',(0.,1.,0.));
#8678=DIRECTION('center_axis',(0.,-1.,0.));
#8679=DIRECTION('ref_axis',(1.,0.,0.));
#8680=DIRECTION('center_axis',(0.,-1.,0.));
#8681=DIRECTION('ref_axis',(1.,0.,0.));
#8682=DIRECTION('center_axis',(0.,1.,0.));
#8683=DIRECTION('ref_axis',(1.,0.,0.));
#8684=DIRECTION('center_axis',(0.,-1.,0.));
#8685=DIRECTION('ref_axis',(0.,0.,-1.));
#8686=DIRECTION('center_axis',(0.,0.,1.));
#8687=DIRECTION('ref_axis',(1.,0.,0.));
#8688=DIRECTION('center_axis',(0.,-1.,0.));
#8689=DIRECTION('ref_axis',(0.,0.,-1.));
#8690=DIRECTION('center_axis',(0.,-1.,0.));
#8691=DIRECTION('ref_axis',(-1.,0.,0.));
#8692=DIRECTION('center_axis',(0.,1.,0.));
#8693=DIRECTION('ref_axis',(1.,0.,0.));
#8694=DIRECTION('axis',(0.,0.,1.));
#8695=DIRECTION('refdir',(1.,0.,0.));
#8696=DIRECTION('center_axis',(0.,1.,0.));
#8697=DIRECTION('ref_axis',(0.,0.,1.));
#8698=DIRECTION('center_axis',(0.,-1.,0.));
#8699=DIRECTION('ref_axis',(1.,0.,0.));
#8700=DIRECTION('center_axis',(0.,-1.,0.));
#8701=DIRECTION('ref_axis',(1.,0.,0.));
#8702=DIRECTION('center_axis',(0.,-1.,0.));
#8703=DIRECTION('ref_axis',(1.,0.,0.));
#8704=DIRECTION('center_axis',(0.,-1.,0.));
#8705=DIRECTION('ref_axis',(1.,0.,0.));
#8706=DIRECTION('',(0.,1.,0.));
#8707=DIRECTION('center_axis',(0.,-1.,0.));
#8708=DIRECTION('ref_axis',(0.,0.,-1.));
#8709=DIRECTION('center_axis',(0.,-1.,0.));
#8710=DIRECTION('ref_axis',(1.,0.,0.));
#8711=DIRECTION('center_axis',(0.,-1.,0.));
#8712=DIRECTION('ref_axis',(1.,0.,0.));
#8713=DIRECTION('',(0.,1.,0.));
#8714=DIRECTION('center_axis',(0.,1.,0.));
#8715=DIRECTION('ref_axis',(0.,0.,1.));
#8716=DIRECTION('center_axis',(0.,-1.,0.));
#8717=DIRECTION('ref_axis',(1.,0.,0.));
#8718=DIRECTION('center_axis',(0.,-1.,0.));
#8719=DIRECTION('ref_axis',(1.,0.,0.));
#8720=DIRECTION('center_axis',(0.,-1.,0.));
#8721=DIRECTION('ref_axis',(1.,0.,0.));
#8722=DIRECTION('center_axis',(0.,-1.,0.));
#8723=DIRECTION('ref_axis',(1.,0.,0.));
#8724=DIRECTION('',(0.,1.,0.));
#8725=DIRECTION('center_axis',(0.,-1.,0.));
#8726=DIRECTION('ref_axis',(0.,0.,-1.));
#8727=DIRECTION('center_axis',(0.,-1.,0.));
#8728=DIRECTION('ref_axis',(1.,0.,0.));
#8729=DIRECTION('center_axis',(0.,-1.,0.));
#8730=DIRECTION('ref_axis',(1.,0.,0.));
#8731=DIRECTION('',(0.,1.,0.));
#8732=DIRECTION('',(0.,0.,1.));
#8733=DIRECTION('',(1.,0.,0.));
#8734=DIRECTION('',(0.,0.,1.));
#8735=DIRECTION('',(1.,0.,0.));
#8736=DIRECTION('',(0.,0.,1.));
#8737=DIRECTION('',(1.,0.,0.));
#8738=DIRECTION('',(0.,0.,1.));
#8739=DIRECTION('',(1.,0.,0.));
#8740=DIRECTION('',(0.,0.,1.));
#8741=DIRECTION('',(1.,0.,0.));
#8742=DIRECTION('axis',(0.,0.,1.));
#8743=DIRECTION('refdir',(1.,0.,0.));
#8744=DIRECTION('center_axis',(0.,1.,0.));
#8745=DIRECTION('ref_axis',(0.,0.,1.));
#8746=DIRECTION('center_axis',(0.,-1.,0.));
#8747=DIRECTION('ref_axis',(1.,0.,0.));
#8748=DIRECTION('center_axis',(0.,-1.,0.));
#8749=DIRECTION('ref_axis',(1.,0.,0.));
#8750=DIRECTION('center_axis',(0.,-1.,0.));
#8751=DIRECTION('ref_axis',(1.,0.,0.));
#8752=DIRECTION('',(0.707106781186548,0.707106781186547,8.65956056235493E-17));
#8753=DIRECTION('center_axis',(0.,-1.,0.));
#8754=DIRECTION('ref_axis',(1.,0.,0.));
#8755=DIRECTION('center_axis',(0.,-1.,0.));
#8756=DIRECTION('ref_axis',(1.,0.,0.));
#8757=DIRECTION('',(0.,1.,0.));
#8758=DIRECTION('center_axis',(0.,1.,0.));
#8759=DIRECTION('ref_axis',(1.,0.,0.));
#8760=DIRECTION('center_axis',(0.,-1.,0.));
#8761=DIRECTION('ref_axis',(1.,0.,0.));
#8762=DIRECTION('',(-0.707106781186547,0.707106781186548,-8.65956056235493E-17));
#8763=DIRECTION('center_axis',(0.,-1.,0.));
#8764=DIRECTION('ref_axis',(0.,0.,-1.));
#8765=DIRECTION('center_axis',(0.,-1.,0.));
#8766=DIRECTION('ref_axis',(1.,0.,0.));
#8767=DIRECTION('center_axis',(0.,1.,0.));
#8768=DIRECTION('ref_axis',(1.,0.,0.));
#8769=DIRECTION('center_axis',(0.,1.,0.));
#8770=DIRECTION('ref_axis',(1.,0.,0.));
#8771=DIRECTION('',(-0.447213595499958,0.894427190999916,-5.47678698264203E-17));
#8772=DIRECTION('center_axis',(0.,-1.,0.));
#8773=DIRECTION('ref_axis',(1.,0.,0.));
#8774=DIRECTION('center_axis',(0.,1.,0.));
#8775=DIRECTION('ref_axis',(1.,0.,0.));
#8776=DIRECTION('',(0.,1.,0.));
#8777=DIRECTION('center_axis',(0.,1.,0.));
#8778=DIRECTION('ref_axis',(1.,0.,0.));
#8779=DIRECTION('center_axis',(0.,-1.,0.));
#8780=DIRECTION('ref_axis',(1.,0.,0.));
#8781=DIRECTION('',(-0.707106781186547,0.707106781186548,-8.65956056235493E-17));
#8782=DIRECTION('center_axis',(0.,-1.,0.));
#8783=DIRECTION('ref_axis',(0.,0.,-1.));
#8784=DIRECTION('center_axis',(0.866025403784439,0.,-0.5));
#8785=DIRECTION('ref_axis',(0.5,0.,0.866025403784439));
#8786=DIRECTION('',(-0.5,0.,-0.866025403784439));
#8787=DIRECTION('',(0.,-1.,0.));
#8788=DIRECTION('',(0.5,0.,0.866025403784439));
#8789=DIRECTION('',(0.,-1.,0.));
#8790=DIRECTION('center_axis',(1.20185167898973E-16,0.,-1.));
#8791=DIRECTION('ref_axis',(1.,0.,1.20185167898973E-16));
#8792=DIRECTION('',(-1.,0.,-1.20185167898973E-16));
#8793=DIRECTION('',(0.,-1.,0.));
#8794=DIRECTION('',(1.,0.,1.20185167898973E-16));
#8795=DIRECTION('center_axis',(-0.866025403784439,0.,-0.5));
#8796=DIRECTION('ref_axis',(0.5,0.,-0.866025403784439));
#8797=DIRECTION('',(-0.5,0.,0.866025403784439));
#8798=DIRECTION('',(0.,-1.,0.));
#8799=DIRECTION('',(0.5,0.,-0.866025403784439));
#8800=DIRECTION('center_axis',(-0.866025403784439,0.,0.5));
#8801=DIRECTION('ref_axis',(-0.5,0.,-0.866025403784439));
#8802=DIRECTION('',(0.5,0.,0.866025403784439));
#8803=DIRECTION('',(0.,-1.,0.));
#8804=DIRECTION('',(-0.5,0.,-0.866025403784439));
#8805=DIRECTION('center_axis',(-2.40370335797945E-16,0.,1.));
#8806=DIRECTION('ref_axis',(-1.,0.,-2.40370335797945E-16));
#8807=DIRECTION('',(1.,0.,2.40370335797945E-16));
#8808=DIRECTION('',(0.,-1.,0.));
#8809=DIRECTION('',(-1.,0.,-2.40370335797945E-16));
#8810=DIRECTION('center_axis',(0.866025403784439,0.,0.5));
#8811=DIRECTION('ref_axis',(-0.5,0.,0.866025403784439));
#8812=DIRECTION('',(0.5,0.,-0.866025403784439));
#8813=DIRECTION('',(-0.5,0.,0.866025403784439));
#8814=DIRECTION('center_axis',(0.,1.,0.));
#8815=DIRECTION('ref_axis',(1.,0.,0.));
#8816=DIRECTION('center_axis',(0.,-1.,0.));
#8817=DIRECTION('ref_axis',(0.,0.,-1.));
#8818=DIRECTION('axis',(0.,0.,1.));
#8819=DIRECTION('refdir',(1.,0.,0.));
#8820=DIRECTION('axis',(0.,0.,1.));
#8821=DIRECTION('refdir',(1.,0.,0.));
#8822=DIRECTION('center_axis',(0.,1.,0.));
#8823=DIRECTION('ref_axis',(0.,0.,1.));
#8824=DIRECTION('center_axis',(0.,-1.,0.));
#8825=DIRECTION('ref_axis',(1.,0.,0.));
#8826=DIRECTION('',(-1.,0.,0.));
#8827=DIRECTION('',(0.,0.,-1.));
#8828=DIRECTION('',(1.,0.,0.));
#8829=DIRECTION('center_axis',(0.,0.,1.));
#8830=DIRECTION('ref_axis',(1.,0.,0.));
#8831=DIRECTION('',(0.,-1.,0.));
#8832=DIRECTION('',(0.,1.,0.));
#8833=DIRECTION('',(-1.,0.,0.));
#8834=DIRECTION('center_axis',(0.,-1.,0.));
#8835=DIRECTION('ref_axis',(0.,0.,-1.));
#8836=DIRECTION('center_axis',(0.,1.,0.));
#8837=DIRECTION('ref_axis',(1.,0.,0.));
#8838=DIRECTION('',(0.,0.,1.));
#8839=DIRECTION('',(1.,0.,0.));
#8840=DIRECTION('center_axis',(0.,0.,-1.));
#8841=DIRECTION('ref_axis',(-1.,0.,0.));
#8842=DIRECTION('',(0.,1.,0.));
#8843=DIRECTION('',(0.,1.,0.));
#8844=DIRECTION('center_axis',(1.,0.,0.));
#8845=DIRECTION('ref_axis',(0.,0.,-1.));
#8846=DIRECTION('center_axis',(0.,1.,0.));
#8847=DIRECTION('ref_axis',(0.,0.,1.));
#8848=DIRECTION('center_axis',(0.,-1.,0.));
#8849=DIRECTION('ref_axis',(1.,0.,0.));
#8850=DIRECTION('center_axis',(0.,-1.,0.));
#8851=DIRECTION('ref_axis',(1.,0.,0.));
#8852=DIRECTION('center_axis',(0.,-1.,0.));
#8853=DIRECTION('ref_axis',(1.,0.,0.));
#8854=DIRECTION('center_axis',(0.,-1.,0.));
#8855=DIRECTION('ref_axis',(1.,0.,0.));
#8856=DIRECTION('',(0.,1.,0.));
#8857=DIRECTION('center_axis',(0.,-1.,0.));
#8858=DIRECTION('ref_axis',(0.,0.,-1.));
#8859=DIRECTION('center_axis',(0.,-1.,0.));
#8860=DIRECTION('ref_axis',(1.,0.,0.));
#8861=DIRECTION('center_axis',(0.,-1.,0.));
#8862=DIRECTION('ref_axis',(1.,0.,0.));
#8863=DIRECTION('center_axis',(0.,-1.,0.));
#8864=DIRECTION('ref_axis',(1.,0.,0.));
#8865=DIRECTION('',(0.,1.,0.));
#8866=DIRECTION('center_axis',(0.,1.,0.));
#8867=DIRECTION('ref_axis',(0.,0.,1.));
#8868=DIRECTION('center_axis',(0.,-1.,0.));
#8869=DIRECTION('ref_axis',(1.,0.,0.));
#8870=DIRECTION('center_axis',(0.,-1.,0.));
#8871=DIRECTION('ref_axis',(1.,0.,0.));
#8872=DIRECTION('center_axis',(0.,-1.,0.));
#8873=DIRECTION('ref_axis',(1.,0.,0.));
#8874=DIRECTION('',(0.,1.,0.));
#8875=DIRECTION('center_axis',(0.,-1.,0.));
#8876=DIRECTION('ref_axis',(0.,0.,-1.));
#8877=DIRECTION('center_axis',(0.,-1.,0.));
#8878=DIRECTION('ref_axis',(1.,0.,0.));
#8879=DIRECTION('center_axis',(0.,-1.,0.));
#8880=DIRECTION('ref_axis',(1.,0.,0.));
#8881=DIRECTION('center_axis',(0.,-1.,0.));
#8882=DIRECTION('ref_axis',(1.,0.,0.));
#8883=DIRECTION('',(0.,1.,0.));
#8884=DIRECTION('center_axis',(0.,1.,0.));
#8885=DIRECTION('ref_axis',(0.,0.,1.));
#8886=DIRECTION('center_axis',(0.,-1.,0.));
#8887=DIRECTION('ref_axis',(1.,0.,0.));
#8888=DIRECTION('center_axis',(0.,-1.,0.));
#8889=DIRECTION('ref_axis',(1.,0.,0.));
#8890=DIRECTION('center_axis',(0.,-1.,0.));
#8891=DIRECTION('ref_axis',(1.,0.,0.));
#8892=DIRECTION('',(0.,1.,0.));
#8893=DIRECTION('center_axis',(0.,-1.,0.));
#8894=DIRECTION('ref_axis',(0.,0.,-1.));
#8895=DIRECTION('center_axis',(0.,-1.,0.));
#8896=DIRECTION('ref_axis',(1.,0.,0.));
#8897=DIRECTION('center_axis',(0.,-1.,0.));
#8898=DIRECTION('ref_axis',(1.,0.,0.));
#8899=DIRECTION('',(0.,1.,0.));
#8900=DIRECTION('axis',(0.,0.,1.));
#8901=DIRECTION('refdir',(1.,0.,0.));
#8902=DIRECTION('center_axis',(0.,1.,0.));
#8903=DIRECTION('ref_axis',(0.,0.,1.));
#8904=DIRECTION('center_axis',(0.,1.,0.));
#8905=DIRECTION('ref_axis',(1.,0.,0.));
#8906=DIRECTION('',(1.,0.,0.));
#8907=DIRECTION('center_axis',(0.,-1.,0.));
#8908=DIRECTION('ref_axis',(1.,0.,0.));
#8909=DIRECTION('',(-1.,0.,0.));
#8910=DIRECTION('center_axis',(0.,0.,-1.));
#8911=DIRECTION('ref_axis',(-1.,0.,0.));
#8912=DIRECTION('',(0.,-1.,0.));
#8913=DIRECTION('',(0.,1.,0.));
#8914=DIRECTION('',(1.,0.,0.));
#8915=DIRECTION('center_axis',(0.,-1.,0.));
#8916=DIRECTION('ref_axis',(0.,0.,-1.));
#8917=DIRECTION('center_axis',(0.,-1.,0.));
#8918=DIRECTION('ref_axis',(1.,0.,0.));
#8919=DIRECTION('center_axis',(0.,1.,0.));
#8920=DIRECTION('ref_axis',(1.,0.,0.));
#8921=DIRECTION('',(-1.,0.,0.));
#8922=DIRECTION('center_axis',(0.,0.,1.));
#8923=DIRECTION('ref_axis',(1.,0.,0.));
#8924=DIRECTION('',(0.,1.,0.));
#8925=DIRECTION('',(0.,-1.,0.));
#8926=DIRECTION('center_axis',(0.,1.,0.));
#8927=DIRECTION('ref_axis',(0.,0.,1.));
#8928=DIRECTION('center_axis',(0.,-1.,0.));
#8929=DIRECTION('ref_axis',(1.,0.,0.));
#8930=DIRECTION('center_axis',(0.,-1.,0.));
#8931=DIRECTION('ref_axis',(1.,0.,0.));
#8932=DIRECTION('center_axis',(0.,-1.,0.));
#8933=DIRECTION('ref_axis',(1.,0.,0.));
#8934=DIRECTION('center_axis',(0.,-1.,0.));
#8935=DIRECTION('ref_axis',(1.,0.,0.));
#8936=DIRECTION('',(0.,1.,0.));
#8937=DIRECTION('center_axis',(0.,-1.,0.));
#8938=DIRECTION('ref_axis',(0.,0.,-1.));
#8939=DIRECTION('center_axis',(0.,-1.,0.));
#8940=DIRECTION('ref_axis',(1.,0.,0.));
#8941=DIRECTION('center_axis',(0.,-1.,0.));
#8942=DIRECTION('ref_axis',(1.,0.,0.));
#8943=DIRECTION('',(0.,1.,0.));
#8944=DIRECTION('',(0.,0.,1.));
#8945=DIRECTION('',(1.,0.,0.));
#8946=DIRECTION('',(0.,0.,1.));
#8947=DIRECTION('',(1.,0.,0.));
#8948=DIRECTION('axis',(0.,0.,1.));
#8949=DIRECTION('refdir',(1.,0.,0.));
#8950=DIRECTION('center_axis',(0.866025403784439,0.,-0.5));
#8951=DIRECTION('ref_axis',(0.5,0.,0.866025403784439));
#8952=DIRECTION('',(-0.5,0.,-0.866025403784439));
#8953=DIRECTION('',(0.,-1.,0.));
#8954=DIRECTION('',(0.5,0.,0.866025403784439));
#8955=DIRECTION('',(0.,-1.,0.));
#8956=DIRECTION('center_axis',(1.60246890531964E-16,0.,-1.));
#8957=DIRECTION('ref_axis',(1.,0.,1.60246890531964E-16));
#8958=DIRECTION('',(-1.,0.,-1.60246890531964E-16));
#8959=DIRECTION('',(0.,-1.,0.));
#8960=DIRECTION('',(1.,0.,1.60246890531964E-16));
#8961=DIRECTION('center_axis',(-0.866025403784439,0.,-0.5));
#8962=DIRECTION('ref_axis',(0.5,0.,-0.866025403784439));
#8963=DIRECTION('',(-0.5,0.,0.866025403784439));
#8964=DIRECTION('',(0.,-1.,0.));
#8965=DIRECTION('',(0.5,0.,-0.866025403784439));
#8966=DIRECTION('center_axis',(-0.866025403784439,0.,0.5));
#8967=DIRECTION('ref_axis',(-0.5,0.,-0.866025403784439));
#8968=DIRECTION('',(0.5,0.,0.866025403784439));
#8969=DIRECTION('',(0.,-1.,0.));
#8970=DIRECTION('',(-0.5,0.,-0.866025403784439));
#8971=DIRECTION('center_axis',(-1.60246890531964E-16,0.,1.));
#8972=DIRECTION('ref_axis',(-1.,0.,-1.60246890531964E-16));
#8973=DIRECTION('',(1.,0.,1.60246890531964E-16));
#8974=DIRECTION('',(0.,-1.,0.));
#8975=DIRECTION('',(-1.,0.,-1.60246890531964E-16));
#8976=DIRECTION('center_axis',(0.866025403784439,0.,0.5));
#8977=DIRECTION('ref_axis',(-0.5,0.,0.866025403784439));
#8978=DIRECTION('',(0.5,0.,-0.866025403784439));
#8979=DIRECTION('',(-0.5,0.,0.866025403784439));
#8980=DIRECTION('center_axis',(0.,1.,0.));
#8981=DIRECTION('ref_axis',(1.,0.,0.));
#8982=DIRECTION('center_axis',(0.,-1.,0.));
#8983=DIRECTION('ref_axis',(0.,0.,-1.));
#8984=DIRECTION('center_axis',(0.,1.,0.));
#8985=DIRECTION('ref_axis',(1.,0.,0.));
#8986=DIRECTION('center_axis',(0.,1.,0.));
#8987=DIRECTION('ref_axis',(1.,0.,0.));
#8988=DIRECTION('center_axis',(0.,1.,0.));
#8989=DIRECTION('ref_axis',(0.,0.,1.));
#8990=DIRECTION('center_axis',(0.,-1.,0.));
#8991=DIRECTION('ref_axis',(1.,0.,0.));
#8992=DIRECTION('center_axis',(0.,-1.,0.));
#8993=DIRECTION('ref_axis',(1.,0.,0.));
#8994=DIRECTION('center_axis',(0.,-1.,0.));
#8995=DIRECTION('ref_axis',(1.,0.,0.));
#8996=DIRECTION('',(0.707106781186547,0.707106781186548,8.65956056235493E-17));
#8997=DIRECTION('center_axis',(0.,-1.,0.));
#8998=DIRECTION('ref_axis',(1.,0.,0.));
#8999=DIRECTION('center_axis',(0.,-1.,0.));
#9000=DIRECTION('ref_axis',(1.,0.,0.));
#9001=DIRECTION('',(0.,1.,0.));
#9002=DIRECTION('center_axis',(0.,1.,0.));
#9003=DIRECTION('ref_axis',(1.,0.,0.));
#9004=DIRECTION('center_axis',(0.,-1.,0.));
#9005=DIRECTION('ref_axis',(1.,0.,0.));
#9006=DIRECTION('',(-0.707106781186547,0.707106781186548,-8.65956056235493E-17));
#9007=DIRECTION('center_axis',(0.,-1.,0.));
#9008=DIRECTION('ref_axis',(0.,0.,-1.));
#9009=DIRECTION('center_axis',(0.,-1.,0.));
#9010=DIRECTION('ref_axis',(1.,0.,0.));
#9011=DIRECTION('center_axis',(0.,1.,0.));
#9012=DIRECTION('ref_axis',(1.,0.,0.));
#9013=DIRECTION('center_axis',(0.,1.,0.));
#9014=DIRECTION('ref_axis',(1.,0.,0.));
#9015=DIRECTION('',(-0.447213595499958,0.894427190999916,-5.47678698264203E-17));
#9016=DIRECTION('center_axis',(0.,-1.,0.));
#9017=DIRECTION('ref_axis',(1.,0.,0.));
#9018=DIRECTION('',(0.,1.,0.));
#9019=DIRECTION('axis',(0.,0.,1.));
#9020=DIRECTION('refdir',(1.,0.,0.));
#9021=DIRECTION('axis',(0.,0.,1.));
#9022=DIRECTION('refdir',(1.,0.,0.));
#9023=DIRECTION('center_axis',(0.,1.,0.));
#9024=DIRECTION('ref_axis',(1.,0.,0.));
#9025=DIRECTION('center_axis',(0.,1.,0.));
#9026=DIRECTION('ref_axis',(1.,0.,0.));
#9027=DIRECTION('',(0.,1.,0.));
#9028=DIRECTION('center_axis',(0.,-1.,0.));
#9029=DIRECTION('ref_axis',(1.,0.,0.));
#9030=DIRECTION('center_axis',(0.,1.,0.));
#9031=DIRECTION('ref_axis',(1.,0.,0.));
#9032=DIRECTION('center_axis',(0.,1.,0.));
#9033=DIRECTION('ref_axis',(1.,0.,0.));
#9034=DIRECTION('center_axis',(0.,1.,0.));
#9035=DIRECTION('ref_axis',(1.,0.,0.));
#9036=DIRECTION('',(0.,1.,0.));
#9037=DIRECTION('center_axis',(0.,1.,0.));
#9038=DIRECTION('ref_axis',(1.,0.,0.));
#9039=DIRECTION('center_axis',(0.,1.,0.));
#9040=DIRECTION('ref_axis',(1.,0.,0.));
#9041=DIRECTION('center_axis',(-1.,0.,0.));
#9042=DIRECTION('ref_axis',(0.,0.,1.));
#9043=DIRECTION('',(0.,-1.,0.));
#9044=DIRECTION('',(0.,0.,1.));
#9045=DIRECTION('',(0.,1.,0.));
#9046=DIRECTION('',(0.,0.,-1.));
#9047=DIRECTION('center_axis',(0.,1.,0.));
#9048=DIRECTION('ref_axis',(1.,0.,0.));
#9049=DIRECTION('center_axis',(0.,-1.,0.));
#9050=DIRECTION('ref_axis',(1.,0.,0.));
#9051=DIRECTION('',(-1.,0.,0.));
#9052=DIRECTION('',(0.,0.,1.));
#9053=DIRECTION('center_axis',(1.,0.,0.));
#9054=DIRECTION('ref_axis',(0.,0.,-1.));
#9055=DIRECTION('',(0.,1.,0.));
#9056=DIRECTION('',(0.,1.,0.));
#9057=DIRECTION('',(0.,0.,-1.));
#9058=DIRECTION('center_axis',(0.,0.,1.));
#9059=DIRECTION('ref_axis',(1.,0.,0.));
#9060=DIRECTION('',(1.,0.,0.));
#9061=DIRECTION('center_axis',(0.,1.,0.));
#9062=DIRECTION('ref_axis',(0.,0.,1.));
#9063=DIRECTION('center_axis',(0.,1.,0.));
#9064=DIRECTION('ref_axis',(1.,0.,0.));
#9065=DIRECTION('center_axis',(-1.,0.,0.));
#9066=DIRECTION('ref_axis',(0.,0.,1.));
#9067=DIRECTION('',(0.,-1.,0.));
#9068=DIRECTION('',(0.,0.,1.));
#9069=DIRECTION('',(0.,1.,0.));
#9070=DIRECTION('',(0.,0.,-1.));
#9071=DIRECTION('center_axis',(0.,1.,0.));
#9072=DIRECTION('ref_axis',(1.,0.,0.));
#9073=DIRECTION('center_axis',(0.,-1.,0.));
#9074=DIRECTION('ref_axis',(1.,0.,0.));
#9075=DIRECTION('',(-1.,0.,0.));
#9076=DIRECTION('',(0.,0.,1.));
#9077=DIRECTION('center_axis',(1.,0.,0.));
#9078=DIRECTION('ref_axis',(0.,0.,-1.));
#9079=DIRECTION('',(0.,1.,0.));
#9080=DIRECTION('',(0.,1.,0.));
#9081=DIRECTION('',(0.,0.,-1.));
#9082=DIRECTION('center_axis',(0.,0.,1.));
#9083=DIRECTION('ref_axis',(1.,0.,0.));
#9084=DIRECTION('',(1.,0.,0.));
#9085=DIRECTION('center_axis',(0.,1.,0.));
#9086=DIRECTION('ref_axis',(0.,0.,1.));
#9087=DIRECTION('center_axis',(0.,1.,0.));
#9088=DIRECTION('ref_axis',(1.,0.,0.));
#9089=DIRECTION('center_axis',(0.,1.,0.));
#9090=DIRECTION('ref_axis',(1.,0.,0.));
#9091=DIRECTION('center_axis',(0.,1.,0.));
#9092=DIRECTION('ref_axis',(1.,0.,0.));
#9093=DIRECTION('',(0.,-1.,0.));
#9094=DIRECTION('center_axis',(0.,1.,0.));
#9095=DIRECTION('ref_axis',(1.,0.,0.));
#9096=DIRECTION('center_axis',(0.,1.,0.));
#9097=DIRECTION('ref_axis',(1.,0.,0.));
#9098=DIRECTION('center_axis',(0.,1.,0.));
#9099=DIRECTION('ref_axis',(1.,0.,0.));
#9100=DIRECTION('axis',(0.,0.,1.));
#9101=DIRECTION('refdir',(1.,0.,0.));
#9102=DIRECTION('center_axis',(0.,1.,0.));
#9103=DIRECTION('ref_axis',(1.,0.,0.));
#9104=DIRECTION('center_axis',(0.,-1.,0.));
#9105=DIRECTION('ref_axis',(1.,0.,0.));
#9106=DIRECTION('',(0.,-1.,0.));
#9107=DIRECTION('center_axis',(0.,-1.,0.));
#9108=DIRECTION('ref_axis',(1.,0.,0.));
#9109=DIRECTION('center_axis',(0.,1.,0.));
#9110=DIRECTION('ref_axis',(1.,0.,0.));
#9111=DIRECTION('center_axis',(0.,1.,0.));
#9112=DIRECTION('ref_axis',(1.,0.,0.));
#9113=DIRECTION('',(0.,-1.,0.));
#9114=DIRECTION('center_axis',(0.,1.,0.));
#9115=DIRECTION('ref_axis',(1.,0.,0.));
#9116=DIRECTION('center_axis',(0.,1.,0.));
#9117=DIRECTION('ref_axis',(1.,0.,0.));
#9118=DIRECTION('center_axis',(0.,1.,0.));
#9119=DIRECTION('ref_axis',(1.,0.,0.));
#9120=DIRECTION('axis',(0.,0.,1.));
#9121=DIRECTION('refdir',(1.,0.,0.));
#9122=DIRECTION('center_axis',(0.,1.,0.));
#9123=DIRECTION('ref_axis',(1.,0.,0.));
#9124=DIRECTION('center_axis',(0.,-1.,0.));
#9125=DIRECTION('ref_axis',(1.,0.,0.));
#9126=DIRECTION('',(0.,-1.,0.));
#9127=DIRECTION('center_axis',(0.,-1.,0.));
#9128=DIRECTION('ref_axis',(1.,0.,0.));
#9129=DIRECTION('center_axis',(0.,1.,0.));
#9130=DIRECTION('ref_axis',(1.,0.,0.));
#9131=DIRECTION('center_axis',(0.,1.,0.));
#9132=DIRECTION('ref_axis',(1.,0.,0.));
#9133=DIRECTION('',(0.,-1.,0.));
#9134=DIRECTION('center_axis',(0.,1.,0.));
#9135=DIRECTION('ref_axis',(1.,0.,0.));
#9136=DIRECTION('center_axis',(0.,1.,0.));
#9137=DIRECTION('ref_axis',(1.,0.,0.));
#9138=DIRECTION('center_axis',(0.,1.,0.));
#9139=DIRECTION('ref_axis',(1.,0.,0.));
#9140=DIRECTION('axis',(0.,0.,1.));
#9141=DIRECTION('refdir',(1.,0.,0.));
#9142=DIRECTION('center_axis',(0.,1.,0.));
#9143=DIRECTION('ref_axis',(1.,0.,0.));
#9144=DIRECTION('center_axis',(0.,-1.,0.));
#9145=DIRECTION('ref_axis',(1.,0.,0.));
#9146=DIRECTION('',(0.,-1.,0.));
#9147=DIRECTION('center_axis',(0.,-1.,0.));
#9148=DIRECTION('ref_axis',(1.,0.,0.));
#9149=DIRECTION('center_axis',(0.,1.,0.));
#9150=DIRECTION('ref_axis',(1.,0.,0.));
#9151=DIRECTION('center_axis',(0.,1.,0.));
#9152=DIRECTION('ref_axis',(1.,0.,0.));
#9153=DIRECTION('',(0.,-1.,0.));
#9154=DIRECTION('center_axis',(0.,1.,0.));
#9155=DIRECTION('ref_axis',(1.,0.,0.));
#9156=DIRECTION('center_axis',(0.,1.,0.));
#9157=DIRECTION('ref_axis',(1.,0.,0.));
#9158=DIRECTION('center_axis',(0.,1.,0.));
#9159=DIRECTION('ref_axis',(1.,0.,0.));
#9160=DIRECTION('axis',(0.,0.,1.));
#9161=DIRECTION('refdir',(1.,0.,0.));
#9162=DIRECTION('center_axis',(0.,1.,0.));
#9163=DIRECTION('ref_axis',(1.,0.,0.));
#9164=DIRECTION('center_axis',(0.,-1.,0.));
#9165=DIRECTION('ref_axis',(1.,0.,0.));
#9166=DIRECTION('',(0.,-1.,0.));
#9167=DIRECTION('center_axis',(0.,-1.,0.));
#9168=DIRECTION('ref_axis',(1.,0.,0.));
#9169=DIRECTION('center_axis',(0.,1.,0.));
#9170=DIRECTION('ref_axis',(1.,0.,0.));
#9171=DIRECTION('center_axis',(0.,1.,0.));
#9172=DIRECTION('ref_axis',(1.,0.,0.));
#9173=DIRECTION('',(0.,-1.,0.));
#9174=DIRECTION('center_axis',(0.,1.,0.));
#9175=DIRECTION('ref_axis',(1.,0.,0.));
#9176=DIRECTION('center_axis',(0.,1.,0.));
#9177=DIRECTION('ref_axis',(1.,0.,0.));
#9178=DIRECTION('center_axis',(0.,1.,0.));
#9179=DIRECTION('ref_axis',(1.,0.,0.));
#9180=DIRECTION('axis',(0.,0.,1.));
#9181=DIRECTION('refdir',(1.,0.,0.));
#9182=DIRECTION('center_axis',(-1.,0.,0.));
#9183=DIRECTION('ref_axis',(0.,0.,1.));
#9184=DIRECTION('',(0.,0.,1.));
#9185=DIRECTION('',(0.,1.,0.));
#9186=DIRECTION('',(0.,0.,-1.));
#9187=DIRECTION('',(0.,1.,0.));
#9188=DIRECTION('center_axis',(0.,0.,-1.));
#9189=DIRECTION('ref_axis',(-1.,0.,0.));
#9190=DIRECTION('',(-1.,0.,0.));
#9191=DIRECTION('',(0.,1.,0.));
#9192=DIRECTION('',(1.,0.,0.));
#9193=DIRECTION('center_axis',(1.,0.,0.));
#9194=DIRECTION('ref_axis',(0.,0.,-1.));
#9195=DIRECTION('',(0.,0.,-1.));
#9196=DIRECTION('',(0.,-1.,0.));
#9197=DIRECTION('',(0.,0.,1.));
#9198=DIRECTION('center_axis',(0.,1.,0.));
#9199=DIRECTION('ref_axis',(1.,0.,0.));
#9200=DIRECTION('center_axis',(0.,1.,0.));
#9201=DIRECTION('ref_axis',(1.,0.,0.));
#9202=DIRECTION('center_axis',(0.,-1.,0.));
#9203=DIRECTION('ref_axis',(1.,0.,0.));
#9204=DIRECTION('center_axis',(0.,1.,0.));
#9205=DIRECTION('ref_axis',(-1.83697019872103E-16,0.,1.));
#9206=DIRECTION('center_axis',(0.,1.,0.));
#9207=DIRECTION('ref_axis',(1.,0.,0.));
#9208=DIRECTION('center_axis',(0.,1.,0.));
#9209=DIRECTION('ref_axis',(1.,0.,0.));
#9210=DIRECTION('center_axis',(0.,1.,0.));
#9211=DIRECTION('ref_axis',(1.,0.,0.));
#9212=DIRECTION('',(0.,-1.,0.));
#9213=DIRECTION('center_axis',(0.,1.,0.));
#9214=DIRECTION('ref_axis',(1.,0.,0.));
#9215=DIRECTION('center_axis',(0.,1.,0.));
#9216=DIRECTION('ref_axis',(1.,0.,0.));
#9217=DIRECTION('',(0.,-1.,0.));
#9218=DIRECTION('center_axis',(0.,-1.,0.));
#9219=DIRECTION('ref_axis',(1.,0.,0.));
#9220=DIRECTION('center_axis',(0.,1.,0.));
#9221=DIRECTION('ref_axis',(1.,0.,0.));
#9222=DIRECTION('center_axis',(0.,1.,0.));
#9223=DIRECTION('ref_axis',(1.,0.,0.));
#9224=DIRECTION('center_axis',(0.,1.,0.));
#9225=DIRECTION('ref_axis',(1.,0.,0.));
#9226=DIRECTION('',(0.,-1.,0.));
#9227=DIRECTION('center_axis',(0.,1.,0.));
#9228=DIRECTION('ref_axis',(1.,0.,0.));
#9229=DIRECTION('center_axis',(0.,1.,0.));
#9230=DIRECTION('ref_axis',(1.,0.,0.));
#9231=DIRECTION('center_axis',(0.,1.,0.));
#9232=DIRECTION('ref_axis',(1.,0.,0.));
#9233=DIRECTION('axis',(0.,0.,1.));
#9234=DIRECTION('refdir',(1.,0.,0.));
#9235=DIRECTION('center_axis',(0.,1.,0.));
#9236=DIRECTION('ref_axis',(1.,0.,0.));
#9237=DIRECTION('center_axis',(0.,1.,0.));
#9238=DIRECTION('ref_axis',(1.,0.,0.));
#9239=DIRECTION('',(0.,1.,0.));
#9240=DIRECTION('center_axis',(0.,-1.,0.));
#9241=DIRECTION('ref_axis',(1.,0.,0.));
#9242=DIRECTION('center_axis',(-1.,0.,0.));
#9243=DIRECTION('ref_axis',(0.,0.,1.));
#9244=DIRECTION('',(0.,0.,1.));
#9245=DIRECTION('',(0.,1.,0.));
#9246=DIRECTION('',(0.,0.,-1.));
#9247=DIRECTION('',(0.,1.,0.));
#9248=DIRECTION('center_axis',(0.,0.,-1.));
#9249=DIRECTION('ref_axis',(-1.,0.,0.));
#9250=DIRECTION('',(-1.,0.,0.));
#9251=DIRECTION('',(0.,1.,0.));
#9252=DIRECTION('',(1.,0.,0.));
#9253=DIRECTION('center_axis',(1.,0.,0.));
#9254=DIRECTION('ref_axis',(0.,0.,-1.));
#9255=DIRECTION('',(0.,0.,-1.));
#9256=DIRECTION('',(0.,-1.,0.));
#9257=DIRECTION('',(0.,0.,1.));
#9258=DIRECTION('center_axis',(0.,1.,0.));
#9259=DIRECTION('ref_axis',(1.,0.,0.));
#9260=DIRECTION('center_axis',(0.,1.,0.));
#9261=DIRECTION('ref_axis',(1.,0.,0.));
#9262=DIRECTION('center_axis',(0.,-1.,0.));
#9263=DIRECTION('ref_axis',(1.,0.,0.));
#9264=DIRECTION('center_axis',(0.,1.,0.));
#9265=DIRECTION('ref_axis',(-1.83697019872103E-16,0.,1.));
#9266=DIRECTION('center_axis',(0.,-1.,0.));
#9267=DIRECTION('ref_axis',(1.,0.,0.));
#9268=DIRECTION('center_axis',(0.,1.,0.));
#9269=DIRECTION('ref_axis',(1.,0.,0.));
#9270=DIRECTION('',(0.,-1.,0.));
#9271=DIRECTION('center_axis',(0.,1.,0.));
#9272=DIRECTION('ref_axis',(1.,0.,0.));
#9273=DIRECTION('',(0.,1.,0.));
#9274=DIRECTION('center_axis',(0.,1.,0.));
#9275=DIRECTION('ref_axis',(1.,0.,0.));
#9276=DIRECTION('center_axis',(0.,1.,0.));
#9277=DIRECTION('ref_axis',(1.,0.,0.));
#9278=DIRECTION('',(-1.,0.,0.));
#9279=DIRECTION('center_axis',(0.,-1.,0.));
#9280=DIRECTION('ref_axis',(1.,0.,0.));
#9281=DIRECTION('',(1.,0.,0.));
#9282=DIRECTION('center_axis',(0.,0.,1.));
#9283=DIRECTION('ref_axis',(1.,0.,0.));
#9284=DIRECTION('',(1.,0.,0.));
#9285=DIRECTION('',(0.,1.,0.));
#9286=DIRECTION('center_axis',(0.,0.,-1.));
#9287=DIRECTION('ref_axis',(-1.,0.,0.));
#9288=DIRECTION('',(0.,-1.,0.));
#9289=DIRECTION('',(-1.,0.,0.));
#9290=DIRECTION('center_axis',(0.,1.,0.));
#9291=DIRECTION('ref_axis',(0.,0.,1.));
#9292=DIRECTION('center_axis',(0.,1.,0.));
#9293=DIRECTION('ref_axis',(1.,0.,0.));
#9294=DIRECTION('center_axis',(0.,1.,0.));
#9295=DIRECTION('ref_axis',(1.,0.,0.));
#9296=DIRECTION('',(0.,-1.,0.));
#9297=DIRECTION('center_axis',(0.,1.,0.));
#9298=DIRECTION('ref_axis',(1.,0.,0.));
#9299=DIRECTION('center_axis',(0.,1.,0.));
#9300=DIRECTION('ref_axis',(1.,0.,0.));
#9301=DIRECTION('axis',(0.,0.,1.));
#9302=DIRECTION('refdir',(1.,0.,0.));
#9303=DIRECTION('center_axis',(0.,1.,0.));
#9304=DIRECTION('ref_axis',(1.,0.,0.));
#9305=DIRECTION('center_axis',(0.,1.,0.));
#9306=DIRECTION('ref_axis',(1.,0.,0.));
#9307=DIRECTION('',(0.,1.,0.));
#9308=DIRECTION('center_axis',(0.,1.,0.));
#9309=DIRECTION('ref_axis',(1.,0.,0.));
#9310=DIRECTION('center_axis',(0.,1.,0.));
#9311=DIRECTION('ref_axis',(1.,0.,0.));
#9312=DIRECTION('center_axis',(0.,1.,0.));
#9313=DIRECTION('ref_axis',(1.,0.,0.));
#9314=DIRECTION('center_axis',(0.,1.,0.));
#9315=DIRECTION('ref_axis',(1.,0.,0.));
#9316=DIRECTION('',(0.,-1.,0.));
#9317=DIRECTION('center_axis',(0.,1.,0.));
#9318=DIRECTION('ref_axis',(1.,0.,0.));
#9319=DIRECTION('center_axis',(0.,1.,0.));
#9320=DIRECTION('ref_axis',(1.,0.,0.));
#9321=DIRECTION('center_axis',(0.,1.,0.));
#9322=DIRECTION('ref_axis',(1.,0.,0.));
#9323=DIRECTION('axis',(0.,0.,1.));
#9324=DIRECTION('refdir',(1.,0.,0.));
#9325=DIRECTION('center_axis',(0.,1.,0.));
#9326=DIRECTION('ref_axis',(1.,0.,0.));
#9327=DIRECTION('center_axis',(0.,-1.,0.));
#9328=DIRECTION('ref_axis',(1.,0.,0.));
#9329=DIRECTION('',(0.,-1.,0.));
#9330=DIRECTION('center_axis',(0.,-1.,0.));
#9331=DIRECTION('ref_axis',(1.,0.,0.));
#9332=DIRECTION('center_axis',(0.,1.,0.));
#9333=DIRECTION('ref_axis',(1.,0.,0.));
#9334=DIRECTION('center_axis',(0.,1.,0.));
#9335=DIRECTION('ref_axis',(1.,0.,0.));
#9336=DIRECTION('',(0.,-1.,0.));
#9337=DIRECTION('center_axis',(0.,1.,0.));
#9338=DIRECTION('ref_axis',(1.,0.,0.));
#9339=DIRECTION('center_axis',(0.,1.,0.));
#9340=DIRECTION('ref_axis',(1.,0.,0.));
#9341=DIRECTION('center_axis',(0.,1.,0.));
#9342=DIRECTION('ref_axis',(1.,0.,0.));
#9343=DIRECTION('axis',(0.,0.,1.));
#9344=DIRECTION('refdir',(1.,0.,0.));
#9345=DIRECTION('center_axis',(0.,1.,0.));
#9346=DIRECTION('ref_axis',(1.,0.,0.));
#9347=DIRECTION('center_axis',(0.,-1.,0.));
#9348=DIRECTION('ref_axis',(1.,0.,0.));
#9349=DIRECTION('',(0.,-1.,0.));
#9350=DIRECTION('center_axis',(0.,-1.,0.));
#9351=DIRECTION('ref_axis',(1.,0.,0.));
#9352=DIRECTION('center_axis',(0.,1.,0.));
#9353=DIRECTION('ref_axis',(1.,0.,0.));
#9354=DIRECTION('center_axis',(0.,1.,0.));
#9355=DIRECTION('ref_axis',(1.,0.,0.));
#9356=DIRECTION('',(0.,-1.,0.));
#9357=DIRECTION('center_axis',(0.,1.,0.));
#9358=DIRECTION('ref_axis',(1.,0.,0.));
#9359=DIRECTION('center_axis',(0.,1.,0.));
#9360=DIRECTION('ref_axis',(1.,0.,0.));
#9361=DIRECTION('center_axis',(0.,1.,0.));
#9362=DIRECTION('ref_axis',(1.,0.,0.));
#9363=DIRECTION('axis',(0.,0.,1.));
#9364=DIRECTION('refdir',(1.,0.,0.));
#9365=DIRECTION('center_axis',(1.,0.,0.));
#9366=DIRECTION('ref_axis',(0.,0.,-1.));
#9367=DIRECTION('',(0.,0.707106781186547,-0.707106781186548));
#9368=DIRECTION('',(0.,1.,0.));
#9369=DIRECTION('',(0.,0.707106781186547,0.707106781186548));
#9370=DIRECTION('',(0.,0.,1.));
#9371=DIRECTION('',(0.,-0.707106781186548,0.707106781186548));
#9372=DIRECTION('',(0.,-1.,0.));
#9373=DIRECTION('',(0.,-0.707106781186548,-0.707106781186548));
#9374=DIRECTION('',(0.,0.,-1.));
#9375=DIRECTION('center_axis',(0.,-0.707106781186548,-0.707106781186548));
#9376=DIRECTION('ref_axis',(-1.,0.,0.));
#9377=DIRECTION('',(-1.,0.,0.));
#9378=DIRECTION('',(0.,0.707106781186548,-0.707106781186548));
#9379=DIRECTION('',(1.,0.,0.));
#9380=DIRECTION('center_axis',(0.,-1.,0.));
#9381=DIRECTION('ref_axis',(1.,0.,0.));
#9382=DIRECTION('',(1.,0.,0.));
#9383=DIRECTION('',(0.,0.,-1.));
#9384=DIRECTION('center_axis',(0.,-0.707106781186548,0.707106781186547));
#9385=DIRECTION('ref_axis',(1.,0.,0.));
#9386=DIRECTION('',(-1.,0.,0.));
#9387=DIRECTION('',(0.,-0.707106781186547,-0.707106781186548));
#9388=DIRECTION('center_axis',(0.,0.,1.));
#9389=DIRECTION('ref_axis',(1.,0.,0.));
#9390=DIRECTION('',(1.,0.,0.));
#9391=DIRECTION('',(0.,-1.,0.));
#9392=DIRECTION('center_axis',(1.,0.,0.));
#9393=DIRECTION('ref_axis',(0.,0.,-1.));
#9394=DIRECTION('',(0.,-0.707106781186547,0.707106781186548));
#9395=DIRECTION('',(0.,0.,1.));
#9396=DIRECTION('',(0.,0.707106781186548,0.707106781186548));
#9397=DIRECTION('',(0.,1.,0.));
#9398=DIRECTION('center_axis',(0.,0.707106781186548,0.707106781186547));
#9399=DIRECTION('ref_axis',(1.,0.,0.));
#9400=DIRECTION('',(-1.,0.,0.));
#9401=DIRECTION('center_axis',(0.,1.,0.));
#9402=DIRECTION('ref_axis',(-1.,0.,0.));
#9403=DIRECTION('',(1.,0.,0.));
#9404=DIRECTION('center_axis',(0.,0.707106781186548,-0.707106781186548));
#9405=DIRECTION('ref_axis',(-1.,0.,0.));
#9406=DIRECTION('',(-1.,0.,0.));
#9407=DIRECTION('center_axis',(0.,0.,1.));
#9408=DIRECTION('ref_axis',(1.,0.,0.));
#9409=DIRECTION('axis',(0.,0.,1.));
#9410=DIRECTION('refdir',(1.,0.,0.));
#9411=DIRECTION('center_axis',(0.,1.,0.));
#9412=DIRECTION('ref_axis',(0.,0.,1.));
#9413=DIRECTION('center_axis',(0.,-1.,0.));
#9414=DIRECTION('ref_axis',(1.,0.,0.));
#9415=DIRECTION('center_axis',(0.,-1.,0.));
#9416=DIRECTION('ref_axis',(1.,0.,0.));
#9417=DIRECTION('center_axis',(0.,-1.,0.));
#9418=DIRECTION('ref_axis',(1.,0.,0.));
#9419=DIRECTION('',(0.707106781186547,0.707106781186548,8.65956056235493E-17));
#9420=DIRECTION('center_axis',(0.,-1.,0.));
#9421=DIRECTION('ref_axis',(1.,0.,0.));
#9422=DIRECTION('center_axis',(0.,-1.,0.));
#9423=DIRECTION('ref_axis',(1.,0.,0.));
#9424=DIRECTION('',(0.,1.,0.));
#9425=DIRECTION('center_axis',(0.,1.,0.));
#9426=DIRECTION('ref_axis',(1.,0.,0.));
#9427=DIRECTION('center_axis',(0.,-1.,0.));
#9428=DIRECTION('ref_axis',(1.,0.,0.));
#9429=DIRECTION('',(-0.707106781186547,0.707106781186548,-8.65956056235493E-17));
#9430=DIRECTION('center_axis',(0.,-1.,0.));
#9431=DIRECTION('ref_axis',(0.,0.,-1.));
#9432=DIRECTION('center_axis',(0.,-1.,0.));
#9433=DIRECTION('ref_axis',(1.,0.,0.));
#9434=DIRECTION('center_axis',(0.,1.,0.));
#9435=DIRECTION('ref_axis',(1.,0.,0.));
#9436=DIRECTION('center_axis',(0.,1.,0.));
#9437=DIRECTION('ref_axis',(1.,0.,0.));
#9438=DIRECTION('',(-0.447213595499958,0.894427190999916,-5.47678698264203E-17));
#9439=DIRECTION('center_axis',(0.,-1.,0.));
#9440=DIRECTION('ref_axis',(1.,0.,0.));
#9441=DIRECTION('center_axis',(0.,1.,0.));
#9442=DIRECTION('ref_axis',(1.,0.,0.));
#9443=DIRECTION('',(0.,1.,0.));
#9444=DIRECTION('center_axis',(0.,1.,0.));
#9445=DIRECTION('ref_axis',(1.,0.,0.));
#9446=DIRECTION('center_axis',(0.,-1.,0.));
#9447=DIRECTION('ref_axis',(1.,0.,0.));
#9448=DIRECTION('',(-0.707106781186547,0.707106781186548,-8.65956056235493E-17));
#9449=DIRECTION('center_axis',(0.,-1.,0.));
#9450=DIRECTION('ref_axis',(0.,0.,-1.));
#9451=DIRECTION('center_axis',(0.866025403784439,0.,-0.5));
#9452=DIRECTION('ref_axis',(0.5,0.,0.866025403784439));
#9453=DIRECTION('',(-0.5,0.,-0.866025403784439));
#9454=DIRECTION('',(0.,-1.,0.));
#9455=DIRECTION('',(0.5,0.,0.866025403784439));
#9456=DIRECTION('',(0.,-1.,0.));
#9457=DIRECTION('center_axis',(1.60246890531964E-16,0.,-1.));
#9458=DIRECTION('ref_axis',(1.,0.,1.60246890531964E-16));
#9459=DIRECTION('',(-1.,0.,-1.60246890531964E-16));
#9460=DIRECTION('',(0.,-1.,0.));
#9461=DIRECTION('',(1.,0.,1.60246890531964E-16));
#9462=DIRECTION('center_axis',(-0.866025403784439,0.,-0.5));
#9463=DIRECTION('ref_axis',(0.5,0.,-0.866025403784439));
#9464=DIRECTION('',(-0.5,0.,0.866025403784439));
#9465=DIRECTION('',(0.,-1.,0.));
#9466=DIRECTION('',(0.5,0.,-0.866025403784439));
#9467=DIRECTION('center_axis',(-0.866025403784439,0.,0.5));
#9468=DIRECTION('ref_axis',(-0.5,0.,-0.866025403784439));
#9469=DIRECTION('',(0.5,0.,0.866025403784439));
#9470=DIRECTION('',(0.,-1.,0.));
#9471=DIRECTION('',(-0.5,0.,-0.866025403784439));
#9472=DIRECTION('center_axis',(-1.60246890531964E-16,0.,1.));
#9473=DIRECTION('ref_axis',(-1.,0.,-1.60246890531964E-16));
#9474=DIRECTION('',(1.,0.,1.60246890531964E-16));
#9475=DIRECTION('',(0.,-1.,0.));
#9476=DIRECTION('',(-1.,0.,-1.60246890531964E-16));
#9477=DIRECTION('center_axis',(0.866025403784439,0.,0.5));
#9478=DIRECTION('ref_axis',(-0.5,0.,0.866025403784439));
#9479=DIRECTION('',(0.5,0.,-0.866025403784439));
#9480=DIRECTION('',(-0.5,0.,0.866025403784439));
#9481=DIRECTION('center_axis',(0.,1.,0.));
#9482=DIRECTION('ref_axis',(1.,0.,0.));
#9483=DIRECTION('center_axis',(0.,-1.,0.));
#9484=DIRECTION('ref_axis',(0.,0.,-1.));
#9485=DIRECTION('',(0.,0.,1.));
#9486=DIRECTION('',(1.,0.,0.));
#9487=DIRECTION('',(0.,0.,1.));
#9488=DIRECTION('',(1.,0.,0.));
#9489=DIRECTION('',(0.,0.,1.));
#9490=DIRECTION('',(1.,0.,0.));
#9491=DIRECTION('',(0.,0.,1.));
#9492=DIRECTION('',(1.,0.,0.));
#9493=DIRECTION('',(0.,0.,1.));
#9494=DIRECTION('',(1.,0.,0.));
#9495=DIRECTION('',(0.,0.,1.));
#9496=DIRECTION('',(1.,0.,0.));
#9497=DIRECTION('',(0.,0.,1.));
#9498=DIRECTION('',(1.,0.,0.));
#9499=DIRECTION('',(0.,0.,1.));
#9500=DIRECTION('',(1.,0.,0.));
#9501=DIRECTION('',(0.,0.,1.));
#9502=DIRECTION('',(1.,0.,0.));
#9503=DIRECTION('',(0.,0.,1.));
#9504=DIRECTION('',(1.,0.,0.));
#9505=DIRECTION('',(0.,0.,1.));
#9506=DIRECTION('',(1.,0.,0.));
#9507=DIRECTION('',(0.,0.,1.));
#9508=DIRECTION('',(1.,0.,0.));
#9509=DIRECTION('',(0.,0.,1.));
#9510=DIRECTION('',(1.,0.,0.));
#9511=DIRECTION('',(0.,-1.,2.22044604925031E-16));
#9512=DIRECTION('',(1.,0.,0.));
#9513=DIRECTION('',(0.,-1.,2.22044604925031E-16));
#9514=DIRECTION('',(1.,0.,0.));
#9515=DIRECTION('',(0.,0.,1.));
#9516=DIRECTION('',(1.,0.,0.));
#9517=DIRECTION('',(0.,0.,1.));
#9518=DIRECTION('',(-1.,1.22464679914735E-16,0.));
#9519=DIRECTION('',(0.,0.,1.));
#9520=DIRECTION('',(-1.,1.22464679914735E-16,0.));
#9521=DIRECTION('',(0.,0.,1.));
#9522=DIRECTION('',(-1.,1.22464679914735E-16,0.));
#9523=DIRECTION('',(0.,0.,1.));
#9524=DIRECTION('',(-1.,1.22464679914735E-16,0.));
#9525=DIRECTION('',(0.,0.,1.));
#9526=DIRECTION('',(1.,0.,0.));
#9527=DIRECTION('',(0.,0.,1.));
#9528=DIRECTION('',(1.,0.,0.));
#9529=DIRECTION('',(0.,0.,1.));
#9530=DIRECTION('',(1.,0.,0.));
#9531=DIRECTION('',(0.,0.,1.));
#9532=DIRECTION('',(1.,0.,0.));
#9533=DIRECTION('',(0.,-1.,2.22044604925031E-16));
#9534=DIRECTION('',(1.,0.,0.));
#9535=DIRECTION('',(0.,-1.,2.22044604925031E-16));
#9536=DIRECTION('',(1.,0.,0.));
#9537=DIRECTION('',(0.,0.,1.));
#9538=DIRECTION('',(1.,0.,0.));
#9539=DIRECTION('',(0.,0.,1.));
#9540=DIRECTION('',(-1.,1.22464679914735E-16,0.));
#9541=DIRECTION('',(0.,0.,1.));
#9542=DIRECTION('',(-1.,1.22464679914735E-16,0.));
#9543=DIRECTION('',(0.,0.,1.));
#9544=DIRECTION('',(-1.,1.22464679914735E-16,0.));
#9545=DIRECTION('',(0.,0.,1.));
#9546=DIRECTION('',(-1.,1.22464679914735E-16,0.));
#9547=DIRECTION('',(0.,0.,1.));
#9548=DIRECTION('',(1.,0.,0.));
#9549=DIRECTION('',(0.,0.,1.));
#9550=DIRECTION('',(1.,0.,0.));
#9551=DIRECTION('',(0.,0.,1.));
#9552=DIRECTION('',(1.,0.,0.));
#9553=DIRECTION('',(0.,0.,1.));
#9554=DIRECTION('',(1.,0.,0.));
#9555=DIRECTION('',(0.,-1.,2.22044604925031E-16));
#9556=DIRECTION('',(1.,0.,0.));
#9557=DIRECTION('',(0.,-1.,2.22044604925031E-16));
#9558=DIRECTION('',(1.,0.,0.));
#9559=DIRECTION('',(0.,-1.,2.22044604925031E-16));
#9560=DIRECTION('',(1.,0.,0.));
#9561=DIRECTION('',(0.,-1.,2.22044604925031E-16));
#9562=DIRECTION('',(1.,0.,0.));
#9563=DIRECTION('',(0.,-1.,2.22044604925031E-16));
#9564=DIRECTION('',(1.,0.,0.));
#9565=DIRECTION('',(0.,-1.,2.22044604925031E-16));
#9566=DIRECTION('',(1.,0.,0.));
#9567=DIRECTION('',(0.,-1.,2.22044604925031E-16));
#9568=DIRECTION('',(1.,0.,0.));
#9569=DIRECTION('',(0.,-1.,2.22044604925031E-16));
#9570=DIRECTION('',(1.,0.,0.));
#9571=DIRECTION('',(0.,0.,1.));
#9572=DIRECTION('',(1.,0.,0.));
#9573=DIRECTION('',(0.,0.,1.));
#9574=DIRECTION('',(1.,0.,0.));
#9575=DIRECTION('',(0.,0.,1.));
#9576=DIRECTION('',(1.,0.,0.));
#9577=DIRECTION('',(0.,0.,1.));
#9578=DIRECTION('',(1.,0.,0.));
#9579=DIRECTION('',(0.,0.,1.));
#9580=DIRECTION('',(1.,0.,0.));
#9581=DIRECTION('',(0.,0.,1.));
#9582=DIRECTION('',(1.,0.,0.));
#9583=DIRECTION('',(0.,0.,1.));
#9584=DIRECTION('',(1.,0.,0.));
#9585=DIRECTION('',(0.,0.,1.));
#9586=DIRECTION('',(1.,0.,0.));
#9587=DIRECTION('',(0.,0.,1.));
#9588=DIRECTION('',(1.,0.,0.));
#9589=DIRECTION('',(0.,0.,1.));
#9590=DIRECTION('',(1.,0.,0.));
#9591=DIRECTION('',(8.65956056235493E-17,-8.65956056235493E-17,-1.));
#9592=DIRECTION('',(2.22044604925031E-16,1.,-8.65956056235494E-17));
#9593=DIRECTION('',(8.65956056235493E-17,-8.65956056235493E-17,-1.));
#9594=DIRECTION('',(2.22044604925031E-16,1.,-8.65956056235494E-17));
#9595=DIRECTION('',(0.,0.,1.));
#9596=DIRECTION('',(-1.,1.22464679914735E-16,0.));
#9597=DIRECTION('',(0.,0.,1.));
#9598=DIRECTION('',(-1.,1.22464679914735E-16,0.));
#9599=DIRECTION('',(0.,0.,1.));
#9600=DIRECTION('',(1.,0.,0.));
#9601=DIRECTION('axis',(0.,0.,1.));
#9602=DIRECTION('refdir',(1.,0.,0.));
#9603=DIRECTION('axis',(0.,0.,1.));
#9604=DIRECTION('refdir',(1.,0.,0.));
#9605=DIRECTION('center_axis',(0.,0.,1.));
#9606=DIRECTION('ref_axis',(1.,0.,0.));
#9607=DIRECTION('center_axis',(0.,0.,1.));
#9608=DIRECTION('ref_axis',(1.,0.,0.));
#9609=DIRECTION('',(0.,0.,1.));
#9610=DIRECTION('center_axis',(0.,0.,-1.));
#9611=DIRECTION('ref_axis',(1.,0.,0.));
#9612=DIRECTION('center_axis',(0.,1.,0.));
#9613=DIRECTION('ref_axis',(-1.,0.,0.));
#9614=DIRECTION('',(-1.,0.,0.));
#9615=DIRECTION('',(0.,0.,1.));
#9616=DIRECTION('',(-1.,0.,0.));
#9617=DIRECTION('',(0.,0.,1.));
#9618=DIRECTION('center_axis',(1.,0.,0.));
#9619=DIRECTION('ref_axis',(0.,1.,0.));
#9620=DIRECTION('',(0.,1.,0.));
#9621=DIRECTION('',(0.,1.,0.));
#9622=DIRECTION('',(0.,0.,1.));
#9623=DIRECTION('center_axis',(0.,-1.,0.));
#9624=DIRECTION('ref_axis',(1.,0.,0.));
#9625=DIRECTION('',(1.,0.,0.));
#9626=DIRECTION('',(1.,0.,0.));
#9627=DIRECTION('',(0.,0.,1.));
#9628=DIRECTION('center_axis',(-1.,0.,0.));
#9629=DIRECTION('ref_axis',(0.,-1.,0.));
#9630=DIRECTION('',(0.,-1.,0.));
#9631=DIRECTION('',(0.,-1.,0.));
#9632=DIRECTION('center_axis',(0.,0.,1.));
#9633=DIRECTION('ref_axis',(1.,0.,0.));
#9634=DIRECTION('center_axis',(0.,0.,1.));
#9635=DIRECTION('ref_axis',(1.,0.,0.));
#9636=DIRECTION('axis',(0.,0.,1.));
#9637=DIRECTION('refdir',(1.,0.,0.));
#9638=DIRECTION('center_axis',(0.,0.,1.));
#9639=DIRECTION('ref_axis',(1.,0.,0.));
#9640=DIRECTION('center_axis',(0.,0.,1.));
#9641=DIRECTION('ref_axis',(1.,0.,0.));
#9642=DIRECTION('',(0.,0.,1.));
#9643=DIRECTION('center_axis',(0.,0.,-1.));
#9644=DIRECTION('ref_axis',(1.,0.,0.));
#9645=DIRECTION('center_axis',(0.,0.,1.));
#9646=DIRECTION('ref_axis',(1.,0.,0.));
#9647=DIRECTION('center_axis',(0.,0.,1.));
#9648=DIRECTION('ref_axis',(1.,0.,0.));
#9649=DIRECTION('',(0.,0.,1.));
#9650=DIRECTION('center_axis',(0.,0.,-1.));
#9651=DIRECTION('ref_axis',(1.,0.,0.));
#9652=DIRECTION('center_axis',(0.,0.,1.));
#9653=DIRECTION('ref_axis',(1.,0.,0.));
#9654=DIRECTION('center_axis',(0.,0.,1.));
#9655=DIRECTION('ref_axis',(1.,0.,0.));
#9656=DIRECTION('',(0.,0.,1.));
#9657=DIRECTION('center_axis',(0.,0.,-1.));
#9658=DIRECTION('ref_axis',(1.,0.,0.));
#9659=DIRECTION('center_axis',(0.,0.,1.));
#9660=DIRECTION('ref_axis',(1.,0.,0.));
#9661=DIRECTION('center_axis',(0.,0.,1.));
#9662=DIRECTION('ref_axis',(1.,0.,0.));
#9663=DIRECTION('',(0.,0.,1.));
#9664=DIRECTION('center_axis',(0.,0.,-1.));
#9665=DIRECTION('ref_axis',(1.,0.,0.));
#9666=DIRECTION('center_axis',(0.,0.,1.));
#9667=DIRECTION('ref_axis',(1.,0.,0.));
#9668=DIRECTION('',(0.,-1.,0.));
#9669=DIRECTION('',(-1.,0.,0.));
#9670=DIRECTION('',(0.,1.,0.));
#9671=DIRECTION('',(1.,0.,0.));
#9672=DIRECTION('center_axis',(0.,0.,1.));
#9673=DIRECTION('ref_axis',(1.,0.,0.));
#9674=DIRECTION('center_axis',(0.,1.,0.));
#9675=DIRECTION('ref_axis',(-1.,0.,0.));
#9676=DIRECTION('',(0.,0.,1.));
#9677=DIRECTION('',(-1.,0.,0.));
#9678=DIRECTION('',(0.,0.,1.));
#9679=DIRECTION('center_axis',(1.,0.,0.));
#9680=DIRECTION('ref_axis',(0.,1.,0.));
#9681=DIRECTION('',(0.,1.,0.));
#9682=DIRECTION('',(0.,0.,1.));
#9683=DIRECTION('center_axis',(0.,-1.,0.));
#9684=DIRECTION('ref_axis',(1.,0.,0.));
#9685=DIRECTION('',(1.,0.,0.));
#9686=DIRECTION('',(0.,0.,1.));
#9687=DIRECTION('center_axis',(-1.,0.,0.));
#9688=DIRECTION('ref_axis',(0.,-1.,0.));
#9689=DIRECTION('',(0.,-1.,0.));
#9690=DIRECTION('center_axis',(0.,0.,1.));
#9691=DIRECTION('ref_axis',(1.,0.,0.));
#9692=DIRECTION('center_axis',(0.,0.,1.));
#9693=DIRECTION('ref_axis',(1.,0.,0.));
#9694=DIRECTION('center_axis',(0.,0.,1.));
#9695=DIRECTION('ref_axis',(1.,0.,0.));
#9696=DIRECTION('',(0.,0.,-1.));
#9697=DIRECTION('center_axis',(0.,0.,1.));
#9698=DIRECTION('ref_axis',(1.,0.,0.));
#9699=DIRECTION('center_axis',(0.,0.,1.));
#9700=DIRECTION('ref_axis',(1.,0.,0.));
#9701=DIRECTION('center_axis',(0.,0.,1.));
#9702=DIRECTION('ref_axis',(1.,0.,0.));
#9703=DIRECTION('',(0.,0.,-1.));
#9704=DIRECTION('center_axis',(0.,0.,1.));
#9705=DIRECTION('ref_axis',(1.,0.,0.));
#9706=DIRECTION('center_axis',(0.,0.,1.));
#9707=DIRECTION('ref_axis',(1.,0.,0.));
#9708=DIRECTION('axis',(0.,0.,1.));
#9709=DIRECTION('refdir',(1.,0.,0.));
#9710=DIRECTION('center_axis',(0.,0.,1.));
#9711=DIRECTION('ref_axis',(1.,0.,0.));
#9712=DIRECTION('center_axis',(0.,0.,-1.));
#9713=DIRECTION('ref_axis',(1.,0.,0.));
#9714=DIRECTION('',(0.,0.,-1.));
#9715=DIRECTION('center_axis',(0.,0.,-1.));
#9716=DIRECTION('ref_axis',(1.,0.,0.));
#9717=DIRECTION('center_axis',(0.,0.,1.));
#9718=DIRECTION('ref_axis',(1.,0.,0.));
#9719=DIRECTION('center_axis',(0.,0.,1.));
#9720=DIRECTION('ref_axis',(1.,0.,0.));
#9721=DIRECTION('',(0.,0.,-1.));
#9722=DIRECTION('center_axis',(0.,0.,1.));
#9723=DIRECTION('ref_axis',(1.,0.,0.));
#9724=DIRECTION('center_axis',(0.,0.,1.));
#9725=DIRECTION('ref_axis',(1.,0.,0.));
#9726=DIRECTION('center_axis',(0.,0.,1.));
#9727=DIRECTION('ref_axis',(1.,0.,0.));
#9728=DIRECTION('',(0.,0.,1.));
#9729=DIRECTION('',(1.,0.,0.));
#9730=DIRECTION('',(0.,0.,1.));
#9731=DIRECTION('',(1.,0.,0.));
#9732=DIRECTION('',(0.,0.,1.));
#9733=DIRECTION('',(1.,0.,0.));
#9734=DIRECTION('',(0.,0.,1.));
#9735=DIRECTION('',(1.,0.,0.));
#9736=DIRECTION('',(0.,0.,1.));
#9737=DIRECTION('',(1.,0.,0.));
#9738=DIRECTION('',(0.,0.,1.));
#9739=DIRECTION('',(1.,0.,0.));
#9740=CARTESIAN_POINT('',(0.,0.,0.));
#9741=CARTESIAN_POINT('',(0.,0.,0.));
#9742=CARTESIAN_POINT('',(0.,0.,0.));
#9743=CARTESIAN_POINT('Origin',(3.75,0.,-0.1));
#9744=CARTESIAN_POINT('',(3.54,-2.57175827820944E-17,0.));
#9745=CARTESIAN_POINT('Origin',(3.75,0.,0.));
#9746=CARTESIAN_POINT('',(3.54,2.57175827820944E-17,1.));
#9747=CARTESIAN_POINT('',(3.54,-2.57175827820944E-17,-0.1));
#9748=CARTESIAN_POINT('Origin',(3.75,0.,1.));
#9749=CARTESIAN_POINT('Origin',(-3.75,0.,-0.1));
#9750=CARTESIAN_POINT('',(-3.96,-2.57175827820944E-17,0.));
#9751=CARTESIAN_POINT('Origin',(-3.75,0.,0.));
#9752=CARTESIAN_POINT('',(-3.96,2.57175827820944E-17,1.));
#9753=CARTESIAN_POINT('',(-3.96,-2.57175827820944E-17,-0.1));
#9754=CARTESIAN_POINT('Origin',(-3.75,0.,1.));
#9755=CARTESIAN_POINT('Origin',(-3.,2.5,-0.1));
#9756=CARTESIAN_POINT('',(-3.165,2.5,0.));
#9757=CARTESIAN_POINT('Origin',(-3.,2.5,0.));
#9758=CARTESIAN_POINT('',(-3.165,2.5,1.));
#9759=CARTESIAN_POINT('',(-3.165,2.5,-0.1));
#9760=CARTESIAN_POINT('Origin',(-3.,2.5,1.));
#9761=CARTESIAN_POINT('Origin',(3.,2.5,-0.1));
#9762=CARTESIAN_POINT('',(2.835,2.5,0.));
#9763=CARTESIAN_POINT('Origin',(3.,2.5,0.));
#9764=CARTESIAN_POINT('',(2.835,2.5,1.));
#9765=CARTESIAN_POINT('',(2.835,2.5,-0.1));
#9766=CARTESIAN_POINT('Origin',(3.,2.5,1.));
#9767=CARTESIAN_POINT('Origin',(-3.,-2.5,-0.1));
#9768=CARTESIAN_POINT('',(-3.165,-2.5,0.));
#9769=CARTESIAN_POINT('Origin',(-3.,-2.5,0.));
#9770=CARTESIAN_POINT('',(-3.165,-2.5,1.));
#9771=CARTESIAN_POINT('',(-3.165,-2.5,-0.1));
#9772=CARTESIAN_POINT('Origin',(-3.,-2.5,1.));
#9773=CARTESIAN_POINT('Origin',(3.,-2.5,-0.1));
#9774=CARTESIAN_POINT('',(2.835,-2.5,0.));
#9775=CARTESIAN_POINT('Origin',(3.,-2.5,0.));
#9776=CARTESIAN_POINT('',(2.835,-2.5,1.));
#9777=CARTESIAN_POINT('',(2.835,-2.5,-0.1));
#9778=CARTESIAN_POINT('Origin',(3.,-2.5,1.));
#9779=CARTESIAN_POINT('Origin',(-3.5,4.4,0.6));
#9780=CARTESIAN_POINT('',(3.5,4.4,1.));
#9781=CARTESIAN_POINT('',(-3.5,4.4,1.));
#9782=CARTESIAN_POINT('',(-1.75,4.4,1.));
#9783=CARTESIAN_POINT('',(3.5,4.4,0.6));
#9784=CARTESIAN_POINT('',(3.5,4.4,0.6));
#9785=CARTESIAN_POINT('',(-3.5,4.4,0.6));
#9786=CARTESIAN_POINT('',(-3.5,4.4,0.6));
#9787=CARTESIAN_POINT('',(-3.5,4.4,0.6));
#9788=CARTESIAN_POINT('Origin',(-3.5,8.5,0.6));
#9789=CARTESIAN_POINT('',(-3.5,8.5,1.));
#9790=CARTESIAN_POINT('',(-3.5,5.125,1.));
#9791=CARTESIAN_POINT('',(-3.5,8.5,0.6));
#9792=CARTESIAN_POINT('',(-3.5,8.5,0.6));
#9793=CARTESIAN_POINT('',(-3.5,8.5,0.6));
#9794=CARTESIAN_POINT('Origin',(3.5,8.5,0.6));
#9795=CARTESIAN_POINT('',(3.5,8.5,1.));
#9796=CARTESIAN_POINT('',(1.75,8.5,1.));
#9797=CARTESIAN_POINT('',(3.5,8.5,0.6));
#9798=CARTESIAN_POINT('',(3.5,8.5,0.6));
#9799=CARTESIAN_POINT('',(3.5,8.5,0.6));
#9800=CARTESIAN_POINT('Origin',(3.5,4.4,0.6));
#9801=CARTESIAN_POINT('',(3.5,3.075,1.));
#9802=CARTESIAN_POINT('',(3.5,4.4,0.6));
#9803=CARTESIAN_POINT('Origin',(0.,6.45,0.6));
#9804=CARTESIAN_POINT('Origin',(6.,9.,0.));
#9805=CARTESIAN_POINT('',(6.,9.,0.));
#9806=CARTESIAN_POINT('',(-6.,9.,0.));
#9807=CARTESIAN_POINT('',(6.,9.,0.));
#9808=CARTESIAN_POINT('',(-6.,9.,1.));
#9809=CARTESIAN_POINT('',(-6.,9.,0.));
#9810=CARTESIAN_POINT('',(6.,9.,1.));
#9811=CARTESIAN_POINT('',(6.,9.,1.));
#9812=CARTESIAN_POINT('',(6.,9.,0.));
#9813=CARTESIAN_POINT('Origin',(6.,-5.5,0.));
#9814=CARTESIAN_POINT('',(6.,-5.5,0.));
#9815=CARTESIAN_POINT('',(6.,-5.5,0.));
#9816=CARTESIAN_POINT('',(6.,-5.5,1.));
#9817=CARTESIAN_POINT('',(6.,-5.5,1.));
#9818=CARTESIAN_POINT('',(6.,-5.5,0.));
#9819=CARTESIAN_POINT('Origin',(-6.,-5.5,0.));
#9820=CARTESIAN_POINT('',(-6.,-5.5,0.));
#9821=CARTESIAN_POINT('',(-6.,-5.5,0.));
#9822=CARTESIAN_POINT('',(-6.,-5.5,1.));
#9823=CARTESIAN_POINT('',(-6.,-5.5,1.));
#9824=CARTESIAN_POINT('',(-6.,-5.5,0.));
#9825=CARTESIAN_POINT('Origin',(-6.,9.,0.));
#9826=CARTESIAN_POINT('',(-6.,9.,0.));
#9827=CARTESIAN_POINT('',(-6.,9.,1.));
#9828=CARTESIAN_POINT('Origin',(0.,1.75,1.));
#9829=CARTESIAN_POINT('Origin',(0.,1.75,0.));
#9830=CARTESIAN_POINT('',(0.,0.,0.));
#9831=CARTESIAN_POINT('Origin',(-5.,9.,-0.8));
#9832=CARTESIAN_POINT('',(-5.,9.,-0.8));
#9833=CARTESIAN_POINT('',(-6.,9.,-0.8));
#9834=CARTESIAN_POINT('',(-5.,9.,-0.8));
#9835=CARTESIAN_POINT('',(-6.,9.,0.));
#9836=CARTESIAN_POINT('',(-6.,9.,-0.8));
#9837=CARTESIAN_POINT('',(-5.,9.,0.));
#9838=CARTESIAN_POINT('',(-5.,9.,0.));
#9839=CARTESIAN_POINT('',(-5.,9.,-0.8));
#9840=CARTESIAN_POINT('Origin',(-5.,-5.5,-0.8));
#9841=CARTESIAN_POINT('',(-5.,-5.5,-0.8));
#9842=CARTESIAN_POINT('',(-5.,-5.5,-0.8));
#9843=CARTESIAN_POINT('',(-5.,-5.5,0.));
#9844=CARTESIAN_POINT('',(-5.,-5.5,0.));
#9845=CARTESIAN_POINT('',(-5.,-5.5,-0.8));
#9846=CARTESIAN_POINT('Origin',(-6.,-5.5,-0.8));
#9847=CARTESIAN_POINT('',(-6.,-5.5,-0.8));
#9848=CARTESIAN_POINT('',(-6.,-5.5,-0.8));
#9849=CARTESIAN_POINT('',(-6.,-5.5,0.));
#9850=CARTESIAN_POINT('',(-6.,-5.5,0.));
#9851=CARTESIAN_POINT('',(-6.,-5.5,-0.8));
#9852=CARTESIAN_POINT('Origin',(-6.,9.,-0.8));
#9853=CARTESIAN_POINT('',(-6.,9.,-0.8));
#9854=CARTESIAN_POINT('',(-6.,9.,0.));
#9855=CARTESIAN_POINT('Origin',(-5.5,1.75,0.));
#9856=CARTESIAN_POINT('Origin',(-5.5,1.75,-0.8));
#9857=CARTESIAN_POINT('',(0.,0.,0.));
#9858=CARTESIAN_POINT('Origin',(6.,9.,-0.8));
#9859=CARTESIAN_POINT('',(6.,9.,-0.8));
#9860=CARTESIAN_POINT('',(5.,9.,-0.8));
#9861=CARTESIAN_POINT('',(6.,9.,-0.8));
#9862=CARTESIAN_POINT('',(5.,9.,0.));
#9863=CARTESIAN_POINT('',(5.,9.,-0.8));
#9864=CARTESIAN_POINT('',(6.,9.,0.));
#9865=CARTESIAN_POINT('',(6.,9.,0.));
#9866=CARTESIAN_POINT('',(6.,9.,-0.8));
#9867=CARTESIAN_POINT('Origin',(6.,-5.5,-0.8));
#9868=CARTESIAN_POINT('',(6.,-5.5,-0.8));
#9869=CARTESIAN_POINT('',(6.,-5.5,-0.8));
#9870=CARTESIAN_POINT('',(6.,-5.5,0.));
#9871=CARTESIAN_POINT('',(6.,-5.5,0.));
#9872=CARTESIAN_POINT('',(6.,-5.5,-0.8));
#9873=CARTESIAN_POINT('Origin',(5.,-5.5,-0.8));
#9874=CARTESIAN_POINT('',(5.,-5.5,-0.8));
#9875=CARTESIAN_POINT('',(5.,-5.5,-0.8));
#9876=CARTESIAN_POINT('',(5.,-5.5,0.));
#9877=CARTESIAN_POINT('',(5.,-5.5,0.));
#9878=CARTESIAN_POINT('',(5.,-5.5,-0.8));
#9879=CARTESIAN_POINT('Origin',(5.,9.,-0.8));
#9880=CARTESIAN_POINT('',(5.,9.,-0.8));
#9881=CARTESIAN_POINT('',(5.,9.,0.));
#9882=CARTESIAN_POINT('Origin',(5.5,1.75,0.));
#9883=CARTESIAN_POINT('Origin',(5.5,1.75,-0.8));
#9884=CARTESIAN_POINT('',(0.,0.,0.));
#9885=CARTESIAN_POINT('Origin',(-3.,-2.5,0.9));
#9886=CARTESIAN_POINT('',(-3.225,-2.5,1.));
#9887=CARTESIAN_POINT('Origin',(-3.,-2.5,1.));
#9888=CARTESIAN_POINT('',(-3.225,-2.5,1.8));
#9889=CARTESIAN_POINT('',(-3.225,-2.5,0.9));
#9890=CARTESIAN_POINT('Origin',(-3.,-2.5,1.8));
#9891=CARTESIAN_POINT('Origin',(3.,-2.5,0.9));
#9892=CARTESIAN_POINT('',(2.775,-2.5,1.));
#9893=CARTESIAN_POINT('Origin',(3.,-2.5,1.));
#9894=CARTESIAN_POINT('',(2.775,-2.5,1.8));
#9895=CARTESIAN_POINT('',(2.775,-2.5,0.9));
#9896=CARTESIAN_POINT('Origin',(3.,-2.5,1.8));
#9897=CARTESIAN_POINT('Origin',(-1.4142135623731,-3.4,2.58578643762691));
#9898=CARTESIAN_POINT('',(-1.5792135623731,-3.3,2.58578643762691));
#9899=CARTESIAN_POINT('Origin',(-1.4142135623731,-3.3,2.58578643762691));
#9900=CARTESIAN_POINT('',(-1.5792135623731,-1.7,2.58578643762691));
#9901=CARTESIAN_POINT('',(-1.5792135623731,-3.4,2.58578643762691));
#9902=CARTESIAN_POINT('Origin',(-1.4142135623731,-1.7,2.58578643762691));
#9903=CARTESIAN_POINT('Origin',(-1.41421356237309,-3.4,5.41421356237309));
#9904=CARTESIAN_POINT('',(-1.57921356237309,-3.3,5.41421356237309));
#9905=CARTESIAN_POINT('Origin',(-1.41421356237309,-3.3,5.41421356237309));
#9906=CARTESIAN_POINT('',(-1.57921356237309,-1.7,5.41421356237309));
#9907=CARTESIAN_POINT('',(-1.57921356237309,-3.4,5.41421356237309));
#9908=CARTESIAN_POINT('Origin',(-1.41421356237309,-1.7,5.41421356237309));
#9909=CARTESIAN_POINT('Origin',(1.4142135623731,-3.4,5.41421356237309));
#9910=CARTESIAN_POINT('',(1.2492135623731,-3.3,5.41421356237309));
#9911=CARTESIAN_POINT('Origin',(1.4142135623731,-3.3,5.41421356237309));
#9912=CARTESIAN_POINT('',(1.2492135623731,-1.7,5.41421356237309));
#9913=CARTESIAN_POINT('',(1.2492135623731,-3.4,5.41421356237309));
#9914=CARTESIAN_POINT('Origin',(1.4142135623731,-1.7,5.41421356237309));
#9915=CARTESIAN_POINT('Origin',(1.41421356237309,-3.4,2.5857864376269));
#9916=CARTESIAN_POINT('',(1.24921356237309,-3.3,2.5857864376269));
#9917=CARTESIAN_POINT('Origin',(1.41421356237309,-3.3,2.5857864376269));
#9918=CARTESIAN_POINT('',(1.24921356237309,-1.7,2.5857864376269));
#9919=CARTESIAN_POINT('',(1.24921356237309,-3.4,2.5857864376269));
#9920=CARTESIAN_POINT('Origin',(1.41421356237309,-1.7,2.5857864376269));
#9921=CARTESIAN_POINT('Origin',(0.,-3.4,4.));
#9922=CARTESIAN_POINT('',(-1.6,-3.3,4.));
#9923=CARTESIAN_POINT('Origin',(0.,-3.3,4.));
#9924=CARTESIAN_POINT('',(-1.6,-1.7,4.));
#9925=CARTESIAN_POINT('',(-1.6,-3.4,4.));
#9926=CARTESIAN_POINT('Origin',(0.,-1.7,4.));
#9927=CARTESIAN_POINT('Origin',(-3.6,-3.3,1.8));
#9928=CARTESIAN_POINT('',(2.4,-3.3,1.8));
#9929=CARTESIAN_POINT('',(2.4,-1.7,1.8));
#9930=CARTESIAN_POINT('',(2.4,-3.3,1.8));
#9931=CARTESIAN_POINT('',(3.6,-3.3,1.8));
#9932=CARTESIAN_POINT('',(3.6,-3.3,1.8));
#9933=CARTESIAN_POINT('',(3.6,-1.7,1.8));
#9934=CARTESIAN_POINT('',(3.6,-3.3,1.8));
#9935=CARTESIAN_POINT('',(3.6,-1.7,1.8));
#9936=CARTESIAN_POINT('Origin',(-3.6,-3.3,1.8));
#9937=CARTESIAN_POINT('',(-2.4,-1.7,1.8));
#9938=CARTESIAN_POINT('',(-2.4,-3.3,1.8));
#9939=CARTESIAN_POINT('',(-2.4,-2.5,1.8));
#9940=CARTESIAN_POINT('',(-3.6,-1.7,1.8));
#9941=CARTESIAN_POINT('',(3.6,-1.7,1.8));
#9942=CARTESIAN_POINT('',(-3.6,-3.3,1.8));
#9943=CARTESIAN_POINT('',(-3.6,-3.3,1.8));
#9944=CARTESIAN_POINT('',(3.6,-3.3,1.8));
#9945=CARTESIAN_POINT('Origin',(-3.6,-3.3,1.));
#9946=CARTESIAN_POINT('',(-3.6,-3.3,1.));
#9947=CARTESIAN_POINT('',(-3.6,-3.3,1.8));
#9948=CARTESIAN_POINT('',(-3.6,-1.7,1.));
#9949=CARTESIAN_POINT('',(-3.6,-1.7,1.8));
#9950=CARTESIAN_POINT('',(-3.6,-3.3,1.));
#9951=CARTESIAN_POINT('Origin',(3.6,-3.3,1.8));
#9952=CARTESIAN_POINT('',(3.6,-3.3,1.));
#9953=CARTESIAN_POINT('',(3.6,-3.3,1.));
#9954=CARTESIAN_POINT('',(3.6,-1.7,1.));
#9955=CARTESIAN_POINT('',(3.6,-3.3,1.));
#9956=CARTESIAN_POINT('',(3.6,-1.7,1.));
#9957=CARTESIAN_POINT('Origin',(-2.4,-3.3,1.));
#9958=CARTESIAN_POINT('',(2.4,-3.3,6.5));
#9959=CARTESIAN_POINT('',(2.4,-3.3,1.));
#9960=CARTESIAN_POINT('',(-2.4,-3.3,6.5));
#9961=CARTESIAN_POINT('',(-2.4,-3.3,6.5));
#9962=CARTESIAN_POINT('',(-2.4,-3.3,1.));
#9963=CARTESIAN_POINT('',(-3.6,-3.3,1.));
#9964=CARTESIAN_POINT('Origin',(2.4,-3.3,1.));
#9965=CARTESIAN_POINT('',(2.4,-1.7,6.5));
#9966=CARTESIAN_POINT('',(2.4,-1.7,1.));
#9967=CARTESIAN_POINT('',(2.4,-3.3,6.5));
#9968=CARTESIAN_POINT('Origin',(2.4,-1.7,1.));
#9969=CARTESIAN_POINT('',(-2.4,-1.7,6.5));
#9970=CARTESIAN_POINT('',(-2.4,-1.7,1.));
#9971=CARTESIAN_POINT('',(2.4,-1.7,6.5));
#9972=CARTESIAN_POINT('',(-3.6,-1.7,1.));
#9973=CARTESIAN_POINT('Origin',(-2.4,-1.7,1.));
#9974=CARTESIAN_POINT('',(-2.4,-1.7,6.5));
#9975=CARTESIAN_POINT('Origin',(0.,-2.5,6.5));
#9976=CARTESIAN_POINT('Origin',(0.,-2.5,1.));
#9977=CARTESIAN_POINT('',(0.,0.,0.));
#9978=CARTESIAN_POINT('Origin',(-1.4142135623731,-3.6,2.58578643762691));
#9979=CARTESIAN_POINT('',(-1.6392135623731,-3.5,2.58578643762691));
#9980=CARTESIAN_POINT('Origin',(-1.4142135623731,-3.5,2.58578643762691));
#9981=CARTESIAN_POINT('',(-1.6392135623731,-3.3,2.58578643762691));
#9982=CARTESIAN_POINT('',(-1.6392135623731,-3.6,2.58578643762691));
#9983=CARTESIAN_POINT('Origin',(-1.4142135623731,-3.3,2.58578643762691));
#9984=CARTESIAN_POINT('Origin',(-1.41421356237309,-3.6,5.41421356237309));
#9985=CARTESIAN_POINT('',(-1.6392135623731,-3.5,5.41421356237309));
#9986=CARTESIAN_POINT('Origin',(-1.41421356237309,-3.5,5.41421356237309));
#9987=CARTESIAN_POINT('',(-1.6392135623731,-3.3,5.41421356237309));
#9988=CARTESIAN_POINT('',(-1.6392135623731,-3.6,5.41421356237309));
#9989=CARTESIAN_POINT('Origin',(-1.41421356237309,-3.3,5.41421356237309));
#9990=CARTESIAN_POINT('Origin',(1.4142135623731,-3.6,5.41421356237309));
#9991=CARTESIAN_POINT('',(1.1892135623731,-3.5,5.41421356237309));
#9992=CARTESIAN_POINT('Origin',(1.4142135623731,-3.5,5.41421356237309));
#9993=CARTESIAN_POINT('',(1.1892135623731,-3.3,5.41421356237309));
#9994=CARTESIAN_POINT('',(1.1892135623731,-3.6,5.41421356237309));
#9995=CARTESIAN_POINT('Origin',(1.4142135623731,-3.3,5.41421356237309));
#9996=CARTESIAN_POINT('Origin',(1.41421356237309,-3.6,2.5857864376269));
#9997=CARTESIAN_POINT('',(1.18921356237309,-3.5,2.5857864376269));
#9998=CARTESIAN_POINT('Origin',(1.41421356237309,-3.5,2.5857864376269));
#9999=CARTESIAN_POINT('',(1.18921356237309,-3.3,2.5857864376269));
#10000=CARTESIAN_POINT('',(1.18921356237309,-3.6,2.5857864376269));
#10001=CARTESIAN_POINT('Origin',(1.41421356237309,-3.3,2.5857864376269));
#10002=CARTESIAN_POINT('Origin',(0.,-3.3,4.));
#10003=CARTESIAN_POINT('',(-1.59,-3.,4.));
#10004=CARTESIAN_POINT('Origin',(0.,-3.,4.));
#10005=CARTESIAN_POINT('',(-1.59,-3.3,4.));
#10006=CARTESIAN_POINT('',(-1.59,-3.3,4.));
#10007=CARTESIAN_POINT('Origin',(0.,-3.3,4.));
#10008=CARTESIAN_POINT('Origin',(0.,-3.,4.));
#10009=CARTESIAN_POINT('',(-1.005,-3.,4.));
#10010=CARTESIAN_POINT('Origin',(0.,-3.,4.));
#10011=CARTESIAN_POINT('Origin',(0.,-3.5,4.));
#10012=CARTESIAN_POINT('',(-1.005,-3.5,4.));
#10013=CARTESIAN_POINT('',(-1.005,-3.5,4.));
#10014=CARTESIAN_POINT('Origin',(0.,-3.5,4.));
#10015=CARTESIAN_POINT('Origin',(0.,-3.5,4.));
#10016=CARTESIAN_POINT('',(-2.4,-3.3,4.));
#10017=CARTESIAN_POINT('Origin',(0.,-3.3,4.));
#10018=CARTESIAN_POINT('',(-2.4,-3.5,4.));
#10019=CARTESIAN_POINT('',(-2.4,-3.5,4.));
#10020=CARTESIAN_POINT('Origin',(0.,-3.5,4.));
#10021=CARTESIAN_POINT('Origin',(0.,-3.3,4.));
#10022=CARTESIAN_POINT('Origin',(0.,-3.5,4.));
#10023=CARTESIAN_POINT('',(0.,0.,0.));
#10024=CARTESIAN_POINT('Origin',(-1.4142135623731,-1.8,2.58578643762691));
#10025=CARTESIAN_POINT('',(-1.6392135623731,-1.7,2.58578643762691));
#10026=CARTESIAN_POINT('Origin',(-1.4142135623731,-1.7,2.58578643762691));
#10027=CARTESIAN_POINT('',(-1.6392135623731,-1.5,2.58578643762691));
#10028=CARTESIAN_POINT('',(-1.6392135623731,-1.8,2.58578643762691));
#10029=CARTESIAN_POINT('Origin',(-1.4142135623731,-1.5,2.58578643762691));
#10030=CARTESIAN_POINT('Origin',(-1.41421356237309,-1.8,5.41421356237309));
#10031=CARTESIAN_POINT('',(-1.6392135623731,-1.7,5.41421356237309));
#10032=CARTESIAN_POINT('Origin',(-1.41421356237309,-1.7,5.41421356237309));
#10033=CARTESIAN_POINT('',(-1.6392135623731,-1.5,5.41421356237309));
#10034=CARTESIAN_POINT('',(-1.6392135623731,-1.8,5.41421356237309));
#10035=CARTESIAN_POINT('Origin',(-1.41421356237309,-1.5,5.41421356237309));
#10036=CARTESIAN_POINT('Origin',(1.4142135623731,-1.8,5.41421356237309));
#10037=CARTESIAN_POINT('',(1.1892135623731,-1.7,5.41421356237309));
#10038=CARTESIAN_POINT('Origin',(1.4142135623731,-1.7,5.41421356237309));
#10039=CARTESIAN_POINT('',(1.1892135623731,-1.5,5.41421356237309));
#10040=CARTESIAN_POINT('',(1.1892135623731,-1.8,5.41421356237309));
#10041=CARTESIAN_POINT('Origin',(1.4142135623731,-1.5,5.41421356237309));
#10042=CARTESIAN_POINT('Origin',(1.41421356237309,-1.8,2.5857864376269));
#10043=CARTESIAN_POINT('',(1.18921356237309,-1.7,2.5857864376269));
#10044=CARTESIAN_POINT('Origin',(1.41421356237309,-1.7,2.5857864376269));
#10045=CARTESIAN_POINT('',(1.18921356237309,-1.5,2.5857864376269));
#10046=CARTESIAN_POINT('',(1.18921356237309,-1.8,2.5857864376269));
#10047=CARTESIAN_POINT('Origin',(1.41421356237309,-1.5,2.5857864376269));
#10048=CARTESIAN_POINT('Origin',(0.,-2.,4.));
#10049=CARTESIAN_POINT('',(-1.59,-1.7,4.));
#10050=CARTESIAN_POINT('Origin',(0.,-1.7,4.));
#10051=CARTESIAN_POINT('',(-1.59,-2.,4.));
#10052=CARTESIAN_POINT('',(-1.59,-2.,4.));
#10053=CARTESIAN_POINT('Origin',(0.,-2.,4.));
#10054=CARTESIAN_POINT('Origin',(0.,-2.,4.));
#10055=CARTESIAN_POINT('',(-1.005,-2.,4.));
#10056=CARTESIAN_POINT('Origin',(0.,-2.,4.));
#10057=CARTESIAN_POINT('Origin',(0.,-1.7,4.));
#10058=CARTESIAN_POINT('',(-1.005,-1.5,4.));
#10059=CARTESIAN_POINT('Origin',(0.,-1.5,4.));
#10060=CARTESIAN_POINT('',(-1.005,-1.7,4.));
#10061=CARTESIAN_POINT('Origin',(0.,-1.7,4.));
#10062=CARTESIAN_POINT('',(-2.4,-1.5,4.));
#10063=CARTESIAN_POINT('Origin',(0.,-1.5,4.));
#10064=CARTESIAN_POINT('',(-2.4,-1.7,4.));
#10065=CARTESIAN_POINT('',(-2.4,-1.7,4.));
#10066=CARTESIAN_POINT('Origin',(0.,-1.7,4.));
#10067=CARTESIAN_POINT('Origin',(0.,-1.5,4.));
#10068=CARTESIAN_POINT('Origin',(0.,-1.7,4.));
#10069=CARTESIAN_POINT('',(0.,0.,0.));
#10070=CARTESIAN_POINT('Origin',(-3.,2.5,0.9));
#10071=CARTESIAN_POINT('',(-3.225,2.5,1.));
#10072=CARTESIAN_POINT('Origin',(-3.,2.5,1.));
#10073=CARTESIAN_POINT('',(-3.225,2.5,1.8));
#10074=CARTESIAN_POINT('',(-3.225,2.5,0.9));
#10075=CARTESIAN_POINT('Origin',(-3.,2.5,1.8));
#10076=CARTESIAN_POINT('Origin',(3.,2.5,0.9));
#10077=CARTESIAN_POINT('',(2.775,2.5,1.));
#10078=CARTESIAN_POINT('Origin',(3.,2.5,1.));
#10079=CARTESIAN_POINT('',(2.775,2.5,1.8));
#10080=CARTESIAN_POINT('',(2.775,2.5,0.9));
#10081=CARTESIAN_POINT('Origin',(3.,2.5,1.8));
#10082=CARTESIAN_POINT('Origin',(-1.4142135623731,1.6,2.58578643762691));
#10083=CARTESIAN_POINT('',(-1.5792135623731,1.7,2.58578643762691));
#10084=CARTESIAN_POINT('Origin',(-1.4142135623731,1.7,2.58578643762691));
#10085=CARTESIAN_POINT('',(-1.5792135623731,3.3,2.58578643762691));
#10086=CARTESIAN_POINT('',(-1.5792135623731,1.6,2.58578643762691));
#10087=CARTESIAN_POINT('Origin',(-1.4142135623731,3.3,2.58578643762691));
#10088=CARTESIAN_POINT('Origin',(-1.41421356237309,1.6,5.41421356237309));
#10089=CARTESIAN_POINT('',(-1.57921356237309,1.7,5.41421356237309));
#10090=CARTESIAN_POINT('Origin',(-1.41421356237309,1.7,5.41421356237309));
#10091=CARTESIAN_POINT('',(-1.57921356237309,3.3,5.41421356237309));
#10092=CARTESIAN_POINT('',(-1.57921356237309,1.6,5.41421356237309));
#10093=CARTESIAN_POINT('Origin',(-1.41421356237309,3.3,5.41421356237309));
#10094=CARTESIAN_POINT('Origin',(1.4142135623731,1.6,5.41421356237309));
#10095=CARTESIAN_POINT('',(1.2492135623731,1.7,5.41421356237309));
#10096=CARTESIAN_POINT('Origin',(1.4142135623731,1.7,5.41421356237309));
#10097=CARTESIAN_POINT('',(1.2492135623731,3.3,5.41421356237309));
#10098=CARTESIAN_POINT('',(1.2492135623731,1.6,5.41421356237309));
#10099=CARTESIAN_POINT('Origin',(1.4142135623731,3.3,5.41421356237309));
#10100=CARTESIAN_POINT('Origin',(1.41421356237309,1.6,2.5857864376269));
#10101=CARTESIAN_POINT('',(1.24921356237309,1.7,2.5857864376269));
#10102=CARTESIAN_POINT('Origin',(1.41421356237309,1.7,2.5857864376269));
#10103=CARTESIAN_POINT('',(1.24921356237309,3.3,2.5857864376269));
#10104=CARTESIAN_POINT('',(1.24921356237309,1.6,2.5857864376269));
#10105=CARTESIAN_POINT('Origin',(1.41421356237309,3.3,2.5857864376269));
#10106=CARTESIAN_POINT('Origin',(0.,1.6,4.));
#10107=CARTESIAN_POINT('',(-1.6,1.7,4.));
#10108=CARTESIAN_POINT('Origin',(0.,1.7,4.));
#10109=CARTESIAN_POINT('',(-1.6,3.3,4.));
#10110=CARTESIAN_POINT('',(-1.6,1.6,4.));
#10111=CARTESIAN_POINT('Origin',(0.,3.3,4.));
#10112=CARTESIAN_POINT('Origin',(-3.6,1.7,1.8));
#10113=CARTESIAN_POINT('',(2.4,1.7,1.8));
#10114=CARTESIAN_POINT('',(2.4,3.3,1.8));
#10115=CARTESIAN_POINT('',(2.4,1.7,1.8));
#10116=CARTESIAN_POINT('',(3.6,1.7,1.8));
#10117=CARTESIAN_POINT('',(3.6,1.7,1.8));
#10118=CARTESIAN_POINT('',(3.6,3.3,1.8));
#10119=CARTESIAN_POINT('',(3.6,1.7,1.8));
#10120=CARTESIAN_POINT('',(3.6,3.3,1.8));
#10121=CARTESIAN_POINT('Origin',(-3.6,1.7,1.8));
#10122=CARTESIAN_POINT('',(-2.4,3.3,1.8));
#10123=CARTESIAN_POINT('',(-2.4,1.7,1.8));
#10124=CARTESIAN_POINT('',(-2.4,2.5,1.8));
#10125=CARTESIAN_POINT('',(-3.6,3.3,1.8));
#10126=CARTESIAN_POINT('',(3.6,3.3,1.8));
#10127=CARTESIAN_POINT('',(-3.6,1.7,1.8));
#10128=CARTESIAN_POINT('',(-3.6,1.7,1.8));
#10129=CARTESIAN_POINT('',(3.6,1.7,1.8));
#10130=CARTESIAN_POINT('Origin',(-3.6,1.7,1.));
#10131=CARTESIAN_POINT('',(-3.6,1.7,1.));
#10132=CARTESIAN_POINT('',(-3.6,1.7,1.8));
#10133=CARTESIAN_POINT('',(-3.6,3.3,1.));
#10134=CARTESIAN_POINT('',(-3.6,3.3,1.8));
#10135=CARTESIAN_POINT('',(-3.6,1.7,1.));
#10136=CARTESIAN_POINT('Origin',(3.6,1.7,1.8));
#10137=CARTESIAN_POINT('',(3.6,1.7,1.));
#10138=CARTESIAN_POINT('',(3.6,1.7,1.));
#10139=CARTESIAN_POINT('',(3.6,3.3,1.));
#10140=CARTESIAN_POINT('',(3.6,1.7,1.));
#10141=CARTESIAN_POINT('',(3.6,3.3,1.));
#10142=CARTESIAN_POINT('Origin',(-2.4,1.7,1.));
#10143=CARTESIAN_POINT('',(2.4,1.7,6.5));
#10144=CARTESIAN_POINT('',(2.4,1.7,1.));
#10145=CARTESIAN_POINT('',(-2.4,1.7,6.5));
#10146=CARTESIAN_POINT('',(-2.4,1.7,6.5));
#10147=CARTESIAN_POINT('',(-2.4,1.7,1.));
#10148=CARTESIAN_POINT('',(-3.6,1.7,1.));
#10149=CARTESIAN_POINT('Origin',(2.4,1.7,1.));
#10150=CARTESIAN_POINT('',(2.4,3.3,6.5));
#10151=CARTESIAN_POINT('',(2.4,3.3,1.));
#10152=CARTESIAN_POINT('',(2.4,1.7,6.5));
#10153=CARTESIAN_POINT('Origin',(2.4,3.3,1.));
#10154=CARTESIAN_POINT('',(-2.4,3.3,6.5));
#10155=CARTESIAN_POINT('',(-2.4,3.3,1.));
#10156=CARTESIAN_POINT('',(2.4,3.3,6.5));
#10157=CARTESIAN_POINT('',(-3.6,3.3,1.));
#10158=CARTESIAN_POINT('Origin',(-2.4,3.3,1.));
#10159=CARTESIAN_POINT('',(-2.4,3.3,6.5));
#10160=CARTESIAN_POINT('Origin',(0.,2.5,6.5));
#10161=CARTESIAN_POINT('Origin',(0.,2.5,1.));
#10162=CARTESIAN_POINT('',(0.,0.,0.));
#10163=CARTESIAN_POINT('Origin',(-1.4142135623731,1.4,2.58578643762691));
#10164=CARTESIAN_POINT('',(-1.6392135623731,1.5,2.58578643762691));
#10165=CARTESIAN_POINT('Origin',(-1.4142135623731,1.5,2.58578643762691));
#10166=CARTESIAN_POINT('',(-1.6392135623731,1.7,2.58578643762691));
#10167=CARTESIAN_POINT('',(-1.6392135623731,1.4,2.58578643762691));
#10168=CARTESIAN_POINT('Origin',(-1.4142135623731,1.7,2.58578643762691));
#10169=CARTESIAN_POINT('Origin',(-1.41421356237309,1.4,5.41421356237309));
#10170=CARTESIAN_POINT('',(-1.6392135623731,1.5,5.41421356237309));
#10171=CARTESIAN_POINT('Origin',(-1.41421356237309,1.5,5.41421356237309));
#10172=CARTESIAN_POINT('',(-1.6392135623731,1.7,5.41421356237309));
#10173=CARTESIAN_POINT('',(-1.6392135623731,1.4,5.41421356237309));
#10174=CARTESIAN_POINT('Origin',(-1.41421356237309,1.7,5.41421356237309));
#10175=CARTESIAN_POINT('Origin',(1.4142135623731,1.4,5.41421356237309));
#10176=CARTESIAN_POINT('',(1.1892135623731,1.5,5.41421356237309));
#10177=CARTESIAN_POINT('Origin',(1.4142135623731,1.5,5.41421356237309));
#10178=CARTESIAN_POINT('',(1.1892135623731,1.7,5.41421356237309));
#10179=CARTESIAN_POINT('',(1.1892135623731,1.4,5.41421356237309));
#10180=CARTESIAN_POINT('Origin',(1.4142135623731,1.7,5.41421356237309));
#10181=CARTESIAN_POINT('Origin',(1.41421356237309,1.4,2.5857864376269));
#10182=CARTESIAN_POINT('',(1.18921356237309,1.5,2.5857864376269));
#10183=CARTESIAN_POINT('Origin',(1.41421356237309,1.5,2.5857864376269));
#10184=CARTESIAN_POINT('',(1.18921356237309,1.7,2.5857864376269));
#10185=CARTESIAN_POINT('',(1.18921356237309,1.4,2.5857864376269));
#10186=CARTESIAN_POINT('Origin',(1.41421356237309,1.7,2.5857864376269));
#10187=CARTESIAN_POINT('Origin',(0.,1.7,4.));
#10188=CARTESIAN_POINT('',(-1.59,2.,4.));
#10189=CARTESIAN_POINT('Origin',(0.,2.,4.));
#10190=CARTESIAN_POINT('',(-1.59,1.7,4.));
#10191=CARTESIAN_POINT('',(-1.59,1.7,4.));
#10192=CARTESIAN_POINT('Origin',(0.,1.7,4.));
#10193=CARTESIAN_POINT('Origin',(0.,2.,4.));
#10194=CARTESIAN_POINT('',(-1.005,2.,4.));
#10195=CARTESIAN_POINT('Origin',(0.,2.,4.));
#10196=CARTESIAN_POINT('Origin',(0.,1.5,4.));
#10197=CARTESIAN_POINT('',(-1.005,1.5,4.));
#10198=CARTESIAN_POINT('',(-1.005,1.5,4.));
#10199=CARTESIAN_POINT('Origin',(0.,1.5,4.));
#10200=CARTESIAN_POINT('Origin',(0.,1.5,4.));
#10201=CARTESIAN_POINT('',(-2.4,1.7,4.));
#10202=CARTESIAN_POINT('Origin',(0.,1.7,4.));
#10203=CARTESIAN_POINT('',(-2.4,1.5,4.));
#10204=CARTESIAN_POINT('',(-2.4,1.5,4.));
#10205=CARTESIAN_POINT('Origin',(0.,1.5,4.));
#10206=CARTESIAN_POINT('Origin',(0.,1.7,4.));
#10207=CARTESIAN_POINT('Origin',(0.,1.5,4.));
#10208=CARTESIAN_POINT('',(0.,0.,0.));
#10209=CARTESIAN_POINT('Origin',(-1.4142135623731,3.2,2.58578643762691));
#10210=CARTESIAN_POINT('',(-1.6392135623731,3.3,2.58578643762691));
#10211=CARTESIAN_POINT('Origin',(-1.4142135623731,3.3,2.58578643762691));
#10212=CARTESIAN_POINT('',(-1.6392135623731,3.5,2.58578643762691));
#10213=CARTESIAN_POINT('',(-1.6392135623731,3.2,2.58578643762691));
#10214=CARTESIAN_POINT('Origin',(-1.4142135623731,3.5,2.58578643762691));
#10215=CARTESIAN_POINT('Origin',(-1.41421356237309,3.2,5.41421356237309));
#10216=CARTESIAN_POINT('',(-1.6392135623731,3.3,5.41421356237309));
#10217=CARTESIAN_POINT('Origin',(-1.41421356237309,3.3,5.41421356237309));
#10218=CARTESIAN_POINT('',(-1.6392135623731,3.5,5.41421356237309));
#10219=CARTESIAN_POINT('',(-1.6392135623731,3.2,5.41421356237309));
#10220=CARTESIAN_POINT('Origin',(-1.41421356237309,3.5,5.41421356237309));
#10221=CARTESIAN_POINT('Origin',(1.4142135623731,3.2,5.41421356237309));
#10222=CARTESIAN_POINT('',(1.1892135623731,3.3,5.41421356237309));
#10223=CARTESIAN_POINT('Origin',(1.4142135623731,3.3,5.41421356237309));
#10224=CARTESIAN_POINT('',(1.1892135623731,3.5,5.41421356237309));
#10225=CARTESIAN_POINT('',(1.1892135623731,3.2,5.41421356237309));
#10226=CARTESIAN_POINT('Origin',(1.4142135623731,3.5,5.41421356237309));
#10227=CARTESIAN_POINT('Origin',(1.41421356237309,3.2,2.5857864376269));
#10228=CARTESIAN_POINT('',(1.18921356237309,3.3,2.5857864376269));
#10229=CARTESIAN_POINT('Origin',(1.41421356237309,3.3,2.5857864376269));
#10230=CARTESIAN_POINT('',(1.18921356237309,3.5,2.5857864376269));
#10231=CARTESIAN_POINT('',(1.18921356237309,3.2,2.5857864376269));
#10232=CARTESIAN_POINT('Origin',(1.41421356237309,3.5,2.5857864376269));
#10233=CARTESIAN_POINT('Origin',(0.,3.,4.));
#10234=CARTESIAN_POINT('',(-1.59,3.3,4.));
#10235=CARTESIAN_POINT('Origin',(0.,3.3,4.));
#10236=CARTESIAN_POINT('',(-1.59,3.,4.));
#10237=CARTESIAN_POINT('',(-1.59,3.,4.));
#10238=CARTESIAN_POINT('Origin',(0.,3.,4.));
#10239=CARTESIAN_POINT('Origin',(0.,3.,4.));
#10240=CARTESIAN_POINT('',(-1.005,3.,4.));
#10241=CARTESIAN_POINT('Origin',(0.,3.,4.));
#10242=CARTESIAN_POINT('Origin',(0.,3.3,4.));
#10243=CARTESIAN_POINT('',(-1.005,3.5,4.));
#10244=CARTESIAN_POINT('Origin',(0.,3.5,4.));
#10245=CARTESIAN_POINT('',(-1.005,3.3,4.));
#10246=CARTESIAN_POINT('Origin',(0.,3.3,4.));
#10247=CARTESIAN_POINT('',(-2.4,3.5,4.));
#10248=CARTESIAN_POINT('Origin',(0.,3.5,4.));
#10249=CARTESIAN_POINT('',(-2.4,3.3,4.));
#10250=CARTESIAN_POINT('',(-2.4,3.3,4.));
#10251=CARTESIAN_POINT('Origin',(0.,3.3,4.));
#10252=CARTESIAN_POINT('Origin',(0.,3.5,4.));
#10253=CARTESIAN_POINT('Origin',(0.,3.3,4.));
#10254=CARTESIAN_POINT('',(0.,0.,0.));
#10255=CARTESIAN_POINT('Origin',(-1.06066017177982,-1.06066017177982,20.2));
#10256=CARTESIAN_POINT('',(-1.22566017177982,-1.06066017177982,20.2));
#10257=CARTESIAN_POINT('Origin',(-1.06066017177982,-1.06066017177982,20.2));
#10258=CARTESIAN_POINT('',(-1.22566017177982,-1.06066017177982,21.));
#10259=CARTESIAN_POINT('',(-1.22566017177982,-1.06066017177982,20.2));
#10260=CARTESIAN_POINT('Origin',(-1.06066017177982,-1.06066017177982,21.));
#10261=CARTESIAN_POINT('Origin',(-1.06066017177982,-1.06066017177982,20.2));
#10262=CARTESIAN_POINT('Origin',(-1.06066017177982,1.06066017177982,20.2));
#10263=CARTESIAN_POINT('',(-1.22566017177982,1.06066017177982,20.2));
#10264=CARTESIAN_POINT('Origin',(-1.06066017177982,1.06066017177982,20.2));
#10265=CARTESIAN_POINT('',(-1.22566017177982,1.06066017177982,21.));
#10266=CARTESIAN_POINT('',(-1.22566017177982,1.06066017177982,20.2));
#10267=CARTESIAN_POINT('Origin',(-1.06066017177982,1.06066017177982,21.));
#10268=CARTESIAN_POINT('Origin',(-1.06066017177982,1.06066017177982,20.2));
#10269=CARTESIAN_POINT('Origin',(1.06066017177982,1.06066017177982,20.2));
#10270=CARTESIAN_POINT('',(0.895660171779821,1.06066017177982,20.2));
#10271=CARTESIAN_POINT('Origin',(1.06066017177982,1.06066017177982,20.2));
#10272=CARTESIAN_POINT('',(0.895660171779821,1.06066017177982,21.));
#10273=CARTESIAN_POINT('',(0.895660171779821,1.06066017177982,20.2));
#10274=CARTESIAN_POINT('Origin',(1.06066017177982,1.06066017177982,21.));
#10275=CARTESIAN_POINT('Origin',(1.06066017177982,1.06066017177982,20.2));
#10276=CARTESIAN_POINT('Origin',(1.06066017177982,-1.06066017177982,20.2));
#10277=CARTESIAN_POINT('',(0.895660171779821,-1.06066017177982,20.2));
#10278=CARTESIAN_POINT('Origin',(1.06066017177982,-1.06066017177982,20.2));
#10279=CARTESIAN_POINT('',(0.895660171779821,-1.06066017177982,21.));
#10280=CARTESIAN_POINT('',(0.895660171779821,-1.06066017177982,20.2));
#10281=CARTESIAN_POINT('Origin',(1.06066017177982,-1.06066017177982,21.));
#10282=CARTESIAN_POINT('Origin',(1.06066017177982,-1.06066017177982,20.2));
#10283=CARTESIAN_POINT('Origin',(0.,0.,12.5));
#10284=CARTESIAN_POINT('',(-1.05,-1.28587913910472E-16,12.5));
#10285=CARTESIAN_POINT('Origin',(0.,0.,12.5));
#10286=CARTESIAN_POINT('',(-1.05,1.28587913910472E-16,21.));
#10287=CARTESIAN_POINT('',(-1.05,-1.28587913910472E-16,12.5));
#10288=CARTESIAN_POINT('Origin',(0.,0.,21.));
#10289=CARTESIAN_POINT('Origin',(0.,0.,12.5));
#10290=CARTESIAN_POINT('',(-0.625,-7.65404249467096E-17,12.5));
#10291=CARTESIAN_POINT('Origin',(0.,0.,12.5));
#10292=CARTESIAN_POINT('Origin',(0.,0.,10.9));
#10293=CARTESIAN_POINT('',(-0.625,-7.65404249467096E-17,11.));
#10294=CARTESIAN_POINT('Origin',(0.,0.,11.));
#10295=CARTESIAN_POINT('',(-0.625,-7.65404249467096E-17,10.9));
#10296=CARTESIAN_POINT('Origin',(3.75,0.,2.4));
#10297=CARTESIAN_POINT('',(3.25,-6.12323399573677E-17,2.4));
#10298=CARTESIAN_POINT('Origin',(3.75,0.,2.4));
#10299=CARTESIAN_POINT('',(3.25,6.12323399573677E-17,21.));
#10300=CARTESIAN_POINT('',(3.25,-6.12323399573677E-17,2.4));
#10301=CARTESIAN_POINT('Origin',(3.75,0.,21.));
#10302=CARTESIAN_POINT('Origin',(3.75,0.,2.4));
#10303=CARTESIAN_POINT('',(3.475,-3.36777869765523E-17,2.4));
#10304=CARTESIAN_POINT('Origin',(3.75,0.,2.4));
#10305=CARTESIAN_POINT('Origin',(3.75,0.,0.9));
#10306=CARTESIAN_POINT('',(3.475,-3.36777869765523E-17,1.));
#10307=CARTESIAN_POINT('Origin',(3.75,0.,1.));
#10308=CARTESIAN_POINT('',(3.475,-3.36777869765523E-17,0.9));
#10309=CARTESIAN_POINT('Origin',(-3.75,0.,2.4));
#10310=CARTESIAN_POINT('',(-4.25,-6.12323399573677E-17,2.4));
#10311=CARTESIAN_POINT('Origin',(-3.75,0.,2.4));
#10312=CARTESIAN_POINT('',(-4.25,6.12323399573677E-17,21.));
#10313=CARTESIAN_POINT('',(-4.25,-6.12323399573677E-17,2.4));
#10314=CARTESIAN_POINT('Origin',(-3.75,0.,21.));
#10315=CARTESIAN_POINT('Origin',(-3.75,0.,2.4));
#10316=CARTESIAN_POINT('',(-4.025,-3.36777869765522E-17,2.4));
#10317=CARTESIAN_POINT('Origin',(-3.75,0.,2.4));
#10318=CARTESIAN_POINT('Origin',(-3.75,0.,0.9));
#10319=CARTESIAN_POINT('',(-4.025,-3.36777869765522E-17,1.));
#10320=CARTESIAN_POINT('Origin',(-3.75,0.,1.));
#10321=CARTESIAN_POINT('',(-4.025,-3.36777869765522E-17,0.9));
#10322=CARTESIAN_POINT('Origin',(4.5,-2.,11.));
#10323=CARTESIAN_POINT('',(-4.5,1.,11.));
#10324=CARTESIAN_POINT('',(-3.,1.,11.));
#10325=CARTESIAN_POINT('',(0.75,1.,11.));
#10326=CARTESIAN_POINT('',(-4.5,2.,11.));
#10327=CARTESIAN_POINT('',(-4.5,-2.,11.));
#10328=CARTESIAN_POINT('',(4.5,2.,11.));
#10329=CARTESIAN_POINT('',(-4.5,2.,11.));
#10330=CARTESIAN_POINT('',(4.5,1.,11.));
#10331=CARTESIAN_POINT('',(4.5,-2.,11.));
#10332=CARTESIAN_POINT('',(3.,1.,11.));
#10333=CARTESIAN_POINT('',(4.125,1.,11.));
#10334=CARTESIAN_POINT('',(3.,-1.,11.));
#10335=CARTESIAN_POINT('',(3.,-1.5,11.));
#10336=CARTESIAN_POINT('',(4.5,-1.,11.));
#10337=CARTESIAN_POINT('',(4.125,-1.,11.));
#10338=CARTESIAN_POINT('',(4.5,-2.,11.));
#10339=CARTESIAN_POINT('',(4.5,-2.,11.));
#10340=CARTESIAN_POINT('',(-4.5,-2.,11.));
#10341=CARTESIAN_POINT('',(-4.5,-2.,11.));
#10342=CARTESIAN_POINT('',(-4.5,-1.,11.));
#10343=CARTESIAN_POINT('',(-4.5,-2.,11.));
#10344=CARTESIAN_POINT('',(-3.,-1.,11.));
#10345=CARTESIAN_POINT('',(0.,-1.,11.));
#10346=CARTESIAN_POINT('',(-3.,-1.5,11.));
#10347=CARTESIAN_POINT('Origin',(0.,2.,16.));
#10348=CARTESIAN_POINT('',(-4.5,2.,21.));
#10349=CARTESIAN_POINT('',(4.5,2.,21.));
#10350=CARTESIAN_POINT('',(4.5,2.,21.));
#10351=CARTESIAN_POINT('',(4.5,2.,11.));
#10352=CARTESIAN_POINT('',(-4.5,2.,21.));
#10353=CARTESIAN_POINT('Origin',(0.,-2.,16.));
#10354=CARTESIAN_POINT('',(4.5,-2.,21.));
#10355=CARTESIAN_POINT('',(-4.5,-2.,21.));
#10356=CARTESIAN_POINT('',(4.5,-2.,21.));
#10357=CARTESIAN_POINT('',(-4.5,-2.,21.));
#10358=CARTESIAN_POINT('',(4.5,-2.,11.));
#10359=CARTESIAN_POINT('Origin',(3.,-1.,1.));
#10360=CARTESIAN_POINT('',(3.,1.,1.));
#10361=CARTESIAN_POINT('',(3.,1.,21.));
#10362=CARTESIAN_POINT('',(3.,-1.,1.));
#10363=CARTESIAN_POINT('',(3.,-1.,1.));
#10364=CARTESIAN_POINT('',(3.,-1.,21.));
#10365=CARTESIAN_POINT('Origin',(3.75,1.,11.));
#10366=CARTESIAN_POINT('',(4.5,1.,1.));
#10367=CARTESIAN_POINT('',(4.5,1.,1.));
#10368=CARTESIAN_POINT('',(3.,1.,1.));
#10369=CARTESIAN_POINT('Origin',(4.5,-1.,1.));
#10370=CARTESIAN_POINT('',(4.5,-1.,1.));
#10371=CARTESIAN_POINT('',(3.,-1.,1.));
#10372=CARTESIAN_POINT('',(4.5,-1.,1.));
#10373=CARTESIAN_POINT('Origin',(4.5,-1.,21.));
#10374=CARTESIAN_POINT('',(4.5,-1.,1.));
#10375=CARTESIAN_POINT('',(4.5,-1.,21.));
#10376=CARTESIAN_POINT('Origin',(3.75,-1.,11.));
#10377=CARTESIAN_POINT('Origin',(-3.,-1.,1.));
#10378=CARTESIAN_POINT('',(-3.,-1.,1.));
#10379=CARTESIAN_POINT('',(-3.,-1.,1.));
#10380=CARTESIAN_POINT('',(-3.,1.,1.));
#10381=CARTESIAN_POINT('',(-3.,-1.,1.));
#10382=CARTESIAN_POINT('',(-3.,1.,1.));
#10383=CARTESIAN_POINT('Origin',(-4.5,-1.,1.));
#10384=CARTESIAN_POINT('',(-4.5,-1.,1.));
#10385=CARTESIAN_POINT('',(-4.5,-1.,1.));
#10386=CARTESIAN_POINT('',(-4.5,-1.,1.));
#10387=CARTESIAN_POINT('Origin',(-3.,1.,1.));
#10388=CARTESIAN_POINT('',(-4.5,1.,1.));
#10389=CARTESIAN_POINT('',(-3.,1.,1.));
#10390=CARTESIAN_POINT('',(-4.5,1.,1.));
#10391=CARTESIAN_POINT('Origin',(-4.5,1.,1.));
#10392=CARTESIAN_POINT('',(-4.5,1.,1.));
#10393=CARTESIAN_POINT('',(-4.5,-2.,21.));
#10394=CARTESIAN_POINT('Origin',(-3.75,0.,21.));
#10395=CARTESIAN_POINT('Origin',(-3.75,0.,1.));
#10396=CARTESIAN_POINT('',(0.,0.,0.));
#10397=CARTESIAN_POINT('Origin',(0.,0.,15.5));
#10398=CARTESIAN_POINT('',(-0.625,-7.65404249467096E-17,16.5));
#10399=CARTESIAN_POINT('Origin',(0.,0.,16.5));
#10400=CARTESIAN_POINT('',(-0.625,-7.65404249467096E-17,15.5));
#10401=CARTESIAN_POINT('',(-0.625,-7.65404249467096E-17,15.5));
#10402=CARTESIAN_POINT('Origin',(0.,0.,15.5));
#10403=CARTESIAN_POINT('Origin',(0.,0.,15.5));
#10404=CARTESIAN_POINT('',(-1.04,-1.27363267111325E-16,16.5));
#10405=CARTESIAN_POINT('Origin',(0.,0.,16.5));
#10406=CARTESIAN_POINT('',(-1.04,-1.27363267111325E-16,15.5));
#10407=CARTESIAN_POINT('',(-1.04,-1.27363267111325E-16,15.5));
#10408=CARTESIAN_POINT('Origin',(0.,0.,15.5));
#10409=CARTESIAN_POINT('Origin',(0.,0.,16.5));
#10410=CARTESIAN_POINT('Origin',(0.,0.,15.5));
#10411=CARTESIAN_POINT('',(0.,0.,0.));
#10412=CARTESIAN_POINT('Origin',(-1.06066017177982,-1.06066017177982,20.9));
#10413=CARTESIAN_POINT('',(-1.28566017177982,-1.06066017177982,21.));
#10414=CARTESIAN_POINT('Origin',(-1.06066017177982,-1.06066017177982,21.));
#10415=CARTESIAN_POINT('',(-1.28566017177982,-1.06066017177982,21.4));
#10416=CARTESIAN_POINT('',(-1.28566017177982,-1.06066017177982,20.9));
#10417=CARTESIAN_POINT('Origin',(-1.06066017177982,-1.06066017177982,21.4));
#10418=CARTESIAN_POINT('Origin',(-1.06066017177982,1.06066017177982,20.9));
#10419=CARTESIAN_POINT('',(-1.28566017177982,1.06066017177982,21.));
#10420=CARTESIAN_POINT('Origin',(-1.06066017177982,1.06066017177982,21.));
#10421=CARTESIAN_POINT('',(-1.28566017177982,1.06066017177982,21.4));
#10422=CARTESIAN_POINT('',(-1.28566017177982,1.06066017177982,20.9));
#10423=CARTESIAN_POINT('Origin',(-1.06066017177982,1.06066017177982,21.4));
#10424=CARTESIAN_POINT('Origin',(1.06066017177982,1.06066017177982,20.9));
#10425=CARTESIAN_POINT('',(0.835660171779821,1.06066017177982,21.));
#10426=CARTESIAN_POINT('Origin',(1.06066017177982,1.06066017177982,21.));
#10427=CARTESIAN_POINT('',(0.835660171779821,1.06066017177982,21.4));
#10428=CARTESIAN_POINT('',(0.835660171779821,1.06066017177982,20.9));
#10429=CARTESIAN_POINT('Origin',(1.06066017177982,1.06066017177982,21.4));
#10430=CARTESIAN_POINT('Origin',(1.06066017177982,-1.06066017177982,20.9));
#10431=CARTESIAN_POINT('',(0.835660171779821,-1.06066017177982,21.));
#10432=CARTESIAN_POINT('Origin',(1.06066017177982,-1.06066017177982,21.));
#10433=CARTESIAN_POINT('',(0.835660171779821,-1.06066017177982,21.4));
#10434=CARTESIAN_POINT('',(0.835660171779821,-1.06066017177982,20.9));
#10435=CARTESIAN_POINT('Origin',(1.06066017177982,-1.06066017177982,21.4));
#10436=CARTESIAN_POINT('Origin',(0.,0.,19.5));
#10437=CARTESIAN_POINT('',(-1.04,-1.27363267111325E-16,21.));
#10438=CARTESIAN_POINT('Origin',(0.,0.,21.));
#10439=CARTESIAN_POINT('',(-1.04,-1.27363267111325E-16,19.5));
#10440=CARTESIAN_POINT('',(-1.04,-1.27363267111325E-16,19.5));
#10441=CARTESIAN_POINT('Origin',(0.,0.,19.5));
#10442=CARTESIAN_POINT('Origin',(0.,0.,19.5));
#10443=CARTESIAN_POINT('',(-0.625,-7.65404249467096E-17,19.5));
#10444=CARTESIAN_POINT('Origin',(0.,0.,19.5));
#10445=CARTESIAN_POINT('Origin',(0.,0.,21.));
#10446=CARTESIAN_POINT('',(-0.625,-7.65404249467096E-17,21.4));
#10447=CARTESIAN_POINT('Origin',(0.,0.,21.4));
#10448=CARTESIAN_POINT('',(-0.625,-7.65404249467096E-17,21.));
#10449=CARTESIAN_POINT('Origin',(0.,0.,21.));
#10450=CARTESIAN_POINT('',(-1.8,-2.20436423846524E-16,21.4));
#10451=CARTESIAN_POINT('Origin',(0.,0.,21.4));
#10452=CARTESIAN_POINT('',(-1.8,-2.20436423846524E-16,21.));
#10453=CARTESIAN_POINT('',(-1.8,-2.20436423846524E-16,21.));
#10454=CARTESIAN_POINT('Origin',(0.,0.,21.));
#10455=CARTESIAN_POINT('Origin',(0.,0.,21.4));
#10456=CARTESIAN_POINT('Origin',(0.,0.,21.));
#10457=CARTESIAN_POINT('',(0.,0.,0.));
#10458=CARTESIAN_POINT('Ctrl Pts',(0.999999511922295,0.00362556505265694,
7.80008768273634));
#10459=CARTESIAN_POINT('Ctrl Pts',(0.999974254701651,0.191242609375982,
7.80916786923111));
#10460=CARTESIAN_POINT('Ctrl Pts',(0.892341067491657,0.564938782877452,
7.82733932423682));
#10461=CARTESIAN_POINT('Ctrl Pts',(0.456009237357814,0.955278731473674,
7.85465504855182));
#10462=CARTESIAN_POINT('Ctrl Pts',(-0.122182810478375,1.05350592491678,
7.88202502929242));
#10463=CARTESIAN_POINT('Ctrl Pts',(-0.665220911419956,0.828753483606749,
7.90945086692426));
#10464=CARTESIAN_POINT('Ctrl Pts',(-1.00612665101876,0.348504727673495,
7.93693161942117));
#10465=CARTESIAN_POINT('Ctrl Pts',(-1.03937057711115,-0.24065277058934,
7.96446742990799));
#10466=CARTESIAN_POINT('Ctrl Pts',(-0.753506480379588,-0.758233234780652,
7.99205790686499));
#10467=CARTESIAN_POINT('Ctrl Pts',(-0.23507859765888,-1.04495072049649,
8.01970284677932));
#10468=CARTESIAN_POINT('Ctrl Pts',(0.357583215672993,-1.01183827364816,
8.04740190675199));
#10469=CARTESIAN_POINT('Ctrl Pts',(0.842723866190013,-0.667819008067397,
8.07515475263842));
#10470=CARTESIAN_POINT('Ctrl Pts',(1.07090748459127,-0.117361728527591,
8.1029609908626));
#10471=CARTESIAN_POINT('Ctrl Pts',(0.971068313490196,0.471237645030074,
8.13082019638131));
#10472=CARTESIAN_POINT('Ctrl Pts',(0.572615291983895,0.917345600069376,
8.15873190469605));
#10473=CARTESIAN_POINT('Ctrl Pts',(-0.00315068596155565,1.08336827030711,
8.18669561143439));
#10474=CARTESIAN_POINT('Ctrl Pts',(-0.580114085036881,0.917350780124834,
8.21471077684478));
#10475=CARTESIAN_POINT('Ctrl Pts',(-0.966051395769627,0.48549839913134,
8.24173733490367));
#10476=CARTESIAN_POINT('Ctrl Pts',(-1.05781582749726,0.0299567596628159,
8.2636033984339));
#10477=CARTESIAN_POINT('Ctrl Pts',(-1.00496213983024,-0.268439331682945,
8.27819794787177));
#10478=CARTESIAN_POINT('Ctrl Pts',(-0.94403781713285,-0.429519542479439,
8.28654256698954));
#10479=CARTESIAN_POINT('Ctrl Pts',(-0.823382078993268,-0.658140969899007,
8.29906435736913));
#10480=CARTESIAN_POINT('Ctrl Pts',(-0.537625296367964,-0.93706913925231,
8.31786521711992));
#10481=CARTESIAN_POINT('Ctrl Pts',(-0.0238288726443125,-1.08214769701979,
8.34297130007593));
#10482=CARTESIAN_POINT('Ctrl Pts',(0.496636287796273,-0.96271505408145,
8.36811512451513));
#10483=CARTESIAN_POINT('Ctrl Pts',(0.966152438091784,-0.550650417462692,
8.39749297986939));
#10484=CARTESIAN_POINT('Ctrl Pts',(1.13301488484768,0.17354695961988,8.43112871623582));
#10485=CARTESIAN_POINT('Ctrl Pts',(0.759782029367692,0.81792928250629,8.46483592073065));
#10486=CARTESIAN_POINT('Ctrl Pts',(0.18659690053678,1.07520238454981,8.49438045894607));
#10487=CARTESIAN_POINT('Ctrl Pts',(-0.350443601960556,1.03519669411318,
8.51973848476555));
#10488=CARTESIAN_POINT('Ctrl Pts',(-0.766297161890012,0.766560498033478,
8.54301401492018));
#10489=CARTESIAN_POINT('Ctrl Pts',(-1.00188555557132,0.390501874334262,
8.56419748306598));
#10490=CARTESIAN_POINT('Ctrl Pts',(-1.10276576842174,-0.133757727725488,
8.5896418232172));
#10491=CARTESIAN_POINT('Ctrl Pts',(-0.847050948528023,-0.7885712029239,
8.6214918164511));
#10492=CARTESIAN_POINT('Ctrl Pts',(-0.0842079511184448,-1.15633714773807,
8.65978061793639));
#10493=CARTESIAN_POINT('Ctrl Pts',(0.72557322963091,-0.906499072035091,
8.69813561803015));
#10494=CARTESIAN_POINT('Ctrl Pts',(1.15047751535783,-0.171671665185466,
8.73655413319947));
#10495=CARTESIAN_POINT('Ctrl Pts',(0.961273159473049,0.658124915791643,
8.77503338584849));
#10496=CARTESIAN_POINT('Ctrl Pts',(0.375126711265494,1.05675920723847,8.80714766479813));
#10497=CARTESIAN_POINT('Ctrl Pts',(-0.164183045710825,1.07538023554299,
8.8328665668906));
#10498=CARTESIAN_POINT('Ctrl Pts',(-0.588587403918608,0.927569264768944,
8.85431383603483));
#10499=CARTESIAN_POINT('Ctrl Pts',(-0.947989492545562,0.577208917394653,
8.87792434906622));
#10500=CARTESIAN_POINT('Ctrl Pts',(-1.10961450093061,0.0536146968196933,
8.90370345540594));
#10501=CARTESIAN_POINT('Ctrl Pts',(-1.00082022593385,-0.483727092204472,
8.92950382341385));
#10502=CARTESIAN_POINT('Ctrl Pts',(-0.648169490504554,-0.904286310022195,
8.95532452406706));
#10503=CARTESIAN_POINT('Ctrl Pts',(-0.137073525470092,-1.1047399934849,
8.98116461266558));
#10504=CARTESIAN_POINT('Ctrl Pts',(0.362995552358674,-1.04213062048012,
9.0048682588092));
#10505=CARTESIAN_POINT('Ctrl Pts',(0.744903368537152,-0.801138176501351,
9.02642976126975));
#10506=CARTESIAN_POINT('Ctrl Pts',(1.06927029269131,-0.365389501861442,
9.05231612054031));
#10507=CARTESIAN_POINT('Ctrl Pts',(1.12442623960627,0.347295239484755,9.08469656290588));
#10508=CARTESIAN_POINT('Ctrl Pts',(0.676375081319218,0.906916376424927,
9.11710422215215));
#10509=CARTESIAN_POINT('Ctrl Pts',(0.162505682592346,1.08489901523682,9.14304497362832));
#10510=CARTESIAN_POINT('Ctrl Pts',(-0.313134592199748,1.06806757295122,
9.16575116654966));
#10511=CARTESIAN_POINT('Ctrl Pts',(-0.80020652042605,0.79906113083438,9.19171186155256));
#10512=CARTESIAN_POINT('Ctrl Pts',(-1.1030130064212,0.251155630516143,9.22093071361268));
#10513=CARTESIAN_POINT('Ctrl Pts',(-1.06806000491819,-0.374587327913118,
9.25016115867103));
#10514=CARTESIAN_POINT('Ctrl Pts',(-0.772382685892504,-0.790331103336901,
9.27398680631869));
#10515=CARTESIAN_POINT('Ctrl Pts',(-0.369190625906315,-1.03674084848642,
9.29673431868371));
#10516=CARTESIAN_POINT('Ctrl Pts',(0.038576143908095,-1.10885924555696,
9.31623572825941));
#10517=CARTESIAN_POINT('Ctrl Pts',(0.477637122556786,-0.990697811322314,
9.33790778885712));
#10518=CARTESIAN_POINT('Ctrl Pts',(0.806650901305872,-0.74814670656117,
9.35741515109002));
#10519=CARTESIAN_POINT('Ctrl Pts',(1.02427838601106,-0.401712335365787,
9.37692457700679));
#10520=CARTESIAN_POINT('Ctrl Pts',(1.0939769734331,-0.0333100781542004,
9.39480970049716));
#10521=CARTESIAN_POINT('Ctrl Pts',(1.04649131988823,0.301575311206996,9.4110697587252));
#10522=CARTESIAN_POINT('Ctrl Pts',(0.881091959620118,0.67241835967004,9.43058245602211));
#10523=CARTESIAN_POINT('Ctrl Pts',(0.491781434765328,1.02078793932956,9.45497403322699));
#10524=CARTESIAN_POINT('Ctrl Pts',(-0.12690622562046,1.12590240218231,9.48424354952418));
#10525=CARTESIAN_POINT('Ctrl Pts',(-0.609455917268022,0.925702271760676,
9.50863324396813));
#10526=CARTESIAN_POINT('Ctrl Pts',(-0.887901221690915,0.630308788370616,
9.52814330365954));
#10527=CARTESIAN_POINT('Ctrl Pts',(-1.07473168029324,0.269973249594665,
9.54765198252425));
#10528=CARTESIAN_POINT('Ctrl Pts',(-1.10429179277937,-0.251571030257534,
9.57203477138778));
#10529=CARTESIAN_POINT('Ctrl Pts',(-0.800909981683876,-0.800300061810875,
9.60128772802457));
#10530=CARTESIAN_POINT('Ctrl Pts',(-0.252449360054481,-1.10339503360944,
9.63053279474191));
#10531=CARTESIAN_POINT('Ctrl Pts',(0.373097965965379,-1.06824993186655,
9.65976848374119));
#10532=CARTESIAN_POINT('Ctrl Pts',(0.883833752107615,-0.705802685092957,
9.68899331286683));
#10533=CARTESIAN_POINT('Ctrl Pts',(1.12336062251109,-0.127424704798401,
9.71820580950298));
#10534=CARTESIAN_POINT('Ctrl Pts',(1.01851100341375,0.489451283507362,9.7474045069875));
#10535=CARTESIAN_POINT('Ctrl Pts',(0.601719134479875,0.955745657723928,
9.7765879476835));
#10536=CARTESIAN_POINT('Ctrl Pts',(0.00114764771726767,1.12873118183179,
9.80575469579441));
#10537=CARTESIAN_POINT('Ctrl Pts',(-0.599201162150444,0.955775323307818,
9.83490331154648));
#10538=CARTESIAN_POINT('Ctrl Pts',(-0.999441525170258,0.507519999720283,
9.86295352909998));
#10539=CARTESIAN_POINT('Ctrl Pts',(-1.11281367201976,-0.0541281101275826,
9.88990656850941));
#10540=CARTESIAN_POINT('Ctrl Pts',(-0.950656776962806,-0.578991698652294,
9.91576396161208));
#10541=CARTESIAN_POINT('Ctrl Pts',(-0.590339529048702,-0.930637197709755,
9.93944961788225));
#10542=CARTESIAN_POINT('Ctrl Pts',(-0.164606104863989,-1.07875415066616,
9.96096785470298));
#10543=CARTESIAN_POINT('Ctrl Pts',(0.376774813272184,-1.06001813820014,
9.98677462212391));
#10544=CARTESIAN_POINT('Ctrl Pts',(0.846936223245377,-0.740877146125449,
10.0125579187175));
#10545=CARTESIAN_POINT('Ctrl Pts',(1.06107082068352,-0.244205647020787,
10.0383162020965));
#10546=CARTESIAN_POINT('Ctrl Pts',(1.08304241869915,0.294959566025181,10.0640572896683));
#10547=CARTESIAN_POINT('Ctrl Pts',(0.729014765427379,0.91016891175548,10.0962004771028));
#10548=CARTESIAN_POINT('Ctrl Pts',(-0.0857101331349617,1.16113591721249,
10.1347162317012));
#10549=CARTESIAN_POINT('Ctrl Pts',(-0.764643776951617,0.832591967114145,
10.1689000478027));
#10550=CARTESIAN_POINT('Ctrl Pts',(-1.0674640769428,0.273793097090764,10.1987708394967));
#10551=CARTESIAN_POINT('Ctrl Pts',(-1.06731019456222,-0.269314357950732,
10.22434609796));
#10552=CARTESIAN_POINT('Ctrl Pts',(-0.807788715964582,-0.746430097707613,
10.2498922819076));
#10553=CARTESIAN_POINT('Ctrl Pts',(-0.352065023972404,-1.04036411773073,
10.275408603128));
#10554=CARTESIAN_POINT('Ctrl Pts',(0.18806187608402,-1.08063605589285,10.3008942987819));
#10555=CARTESIAN_POINT('Ctrl Pts',(0.609132779330515,-0.890423751871434,
10.3226365334534));
#10556=CARTESIAN_POINT('Ctrl Pts',(0.866237924373777,-0.61783839929423,
10.3406489137734));
#10557=CARTESIAN_POINT('Ctrl Pts',(1.04872505851243,-0.26577216648544,10.3597071335657));
#10558=CARTESIAN_POINT('Ctrl Pts',(1.07750116603121,0.243190015038482,10.3835038803323));
#10559=CARTESIAN_POINT('Ctrl Pts',(0.781688530878207,0.777999980609408,
10.4120173608425));
#10560=CARTESIAN_POINT('Ctrl Pts',(0.247719136142376,1.07295015546241,10.4404872688827));
#10561=CARTESIAN_POINT('Ctrl Pts',(-0.360486616831365,1.03867188015668,
10.4689126947258));
#10562=CARTESIAN_POINT('Ctrl Pts',(-0.856395421979649,0.686612064758622,
10.4972927514314));
#10563=CARTESIAN_POINT('Ctrl Pts',(-1.08862861454113,0.125592182065228,
10.5256265935356));
#10564=CARTESIAN_POINT('Ctrl Pts',(-0.986944606168628,-0.472001059894419,
10.5539134034074));
#10565=CARTESIAN_POINT('Ctrl Pts',(-0.583594151562567,-0.923132799570535,
10.5821523997639));
#10566=CARTESIAN_POINT('Ctrl Pts',(-0.00304950196324622,-1.09023227406354,
10.6103428416619));
#10567=CARTESIAN_POINT('Ctrl Pts',(0.576397100829433,-0.923141572582211,
10.6384840153271));
#10568=CARTESIAN_POINT('Ctrl Pts',(0.977415745977647,-0.474174920735025,
10.666575250779));
#10569=CARTESIAN_POINT('Ctrl Pts',(1.07791854333959,0.118262177227866,10.6946159100158));
#10570=CARTESIAN_POINT('Ctrl Pts',(0.848237687346995,0.672348815808936,
10.7226053954193));
#10571=CARTESIAN_POINT('Ctrl Pts',(0.35987034323251,1.01866632704243,10.750543145368));
#10572=CARTESIAN_POINT('Ctrl Pts',(-0.23677931351889,1.05200727853759,10.7784286311663));
#10573=CARTESIAN_POINT('Ctrl Pts',(-0.758730842080508,0.763346883548158,
10.8062613781485));
#10574=CARTESIAN_POINT('Ctrl Pts',(-1.04655744183574,0.242222537004657,
10.8340409125563));
#10575=CARTESIAN_POINT('Ctrl Pts',(-1.01308793288556,-0.351003613269005,
10.8617668734456));
#10576=CARTESIAN_POINT('Ctrl Pts',(-0.669814425530371,-0.834593746223134,
10.889438771651));
#10577=CARTESIAN_POINT('Ctrl Pts',(-0.122977155730889,-1.06092281666227,
10.9170565165848));
#10578=CARTESIAN_POINT('Ctrl Pts',(0.459284142389985,-0.962004532278344,
10.9446192376113));
#10579=CARTESIAN_POINT('Ctrl Pts',(0.898703292351648,-0.568910379520766,
10.9721279252064));
#10580=CARTESIAN_POINT('Ctrl Pts',(1.0071027576084,-0.192548907318078,10.9904290025552));
#10581=CARTESIAN_POINT('Ctrl Pts',(1.00712819276269,-0.00361011030918905,
10.999573158519));
#10582=CARTESIAN_POINT('Ctrl Pts',(0.977559564599991,0.00362254416133655,
7.80008768273634));
#10583=CARTESIAN_POINT('Ctrl Pts',(0.977534866689631,0.18708488976632,7.80896679240822));
#10584=CARTESIAN_POINT('Ctrl Pts',(0.872322415557346,0.552393922726298,
7.82672927903241));
#10585=CARTESIAN_POINT('Ctrl Pts',(0.445718486862071,0.934060193527018,
7.85343643021417));
#10586=CARTESIAN_POINT('Ctrl Pts',(-0.119636647243807,1.03010841597759,
7.88019745241192));
#10587=CARTESIAN_POINT('Ctrl Pts',(-0.650678967970242,0.810334582562273,
7.90701638678188));
#10588=CARTESIAN_POINT('Ctrl Pts',(-0.984099810756226,0.340647684643633,
7.93389180692065));
#10589=CARTESIAN_POINT('Ctrl Pts',(-1.01663027186777,-0.235634070049338,
7.96082469172386));
#10590=CARTESIAN_POINT('Ctrl Pts',(-0.736984385597307,-0.741986536865251,
7.98781490109356));
#10591=CARTESIAN_POINT('Ctrl Pts',(-0.229735381724658,-1.02253990905577,
8.01486274772683));
#10592=CARTESIAN_POINT('Ctrl Pts',(0.350260356893508,-0.990152762857837,
8.04196828714851));
#10593=CARTESIAN_POINT('Ctrl Pts',(0.825134997145517,-0.653436415065432,
8.06913163396793));
#10594=CARTESIAN_POINT('Ctrl Pts',(1.04855042623966,-0.114534980319938,
8.0963528116897));
#10595=CARTESIAN_POINT('Ctrl Pts',(0.950805881040683,0.461848534559346,
8.12363183217922));
#10596=CARTESIAN_POINT('Ctrl Pts',(0.560550547543524,0.89881493391695,8.15096862326752));
#10597=CARTESIAN_POINT('Ctrl Pts',(-0.00352941556499671,1.06149499328244,
8.17836313496341));
#10598=CARTESIAN_POINT('Ctrl Pts',(-0.568945432596404,0.898829335752363,
8.2058151151295));
#10599=CARTESIAN_POINT('Ctrl Pts',(-0.947276485604154,0.475525661597343,
8.23230571210832));
#10600=CARTESIAN_POINT('Ctrl Pts',(-1.03726714683262,0.0288659729588981,
8.25374377338214));
#10601=CARTESIAN_POINT('Ctrl Pts',(-0.985433969276193,-0.263782787095173,
8.26805657036754));
#10602=CARTESIAN_POINT('Ctrl Pts',(-0.925676430299761,-0.421778753641079,
8.27624126130311));
#10603=CARTESIAN_POINT('Ctrl Pts',(-0.807324773446438,-0.646038667836079,
8.28852379480006));
#10604=CARTESIAN_POINT('Ctrl Pts',(-0.526999308588214,-0.919685240659636,
8.30696610050169));
#10605=CARTESIAN_POINT('Ctrl Pts',(-0.0227868718866388,-1.06208690811312,
8.33160304885951));
#10606=CARTESIAN_POINT('Ctrl Pts',(0.48813066286185,-0.944858682751246,
8.35628380467876));
#10607=CARTESIAN_POINT('Ctrl Pts',(0.949193206679585,-0.540258543297488,
8.38512932713425));
#10608=CARTESIAN_POINT('Ctrl Pts',(1.11316501047521,0.171118961858805,8.41816585508126));
#10609=CARTESIAN_POINT('Ctrl Pts',(0.746415595315959,0.80445351686326,8.45128858999103));
#10610=CARTESIAN_POINT('Ctrl Pts',(0.18282724257968,1.05745094591858,8.48033697773421));
#10611=CARTESIAN_POINT('Ctrl Pts',(-0.345419524449013,1.01812107532715,
8.50527861143673));
#10612=CARTESIAN_POINT('Ctrl Pts',(-0.754611477987093,0.753819380993674,
8.52817815885987));
#10613=CARTESIAN_POINT('Ctrl Pts',(-0.986508596508495,0.383672790215633,
8.54902745839679));
#10614=CARTESIAN_POINT('Ctrl Pts',(-1.08584686716394,-0.132493523343181,
8.57407782842635));
#10615=CARTESIAN_POINT('Ctrl Pts',(-0.834046887505374,-0.777476644629888,
8.60544368069453));
#10616=CARTESIAN_POINT('Ctrl Pts',(-0.0822626488291713,-1.14001853467866,
8.64317523263573));
#10617=CARTESIAN_POINT('Ctrl Pts',(0.716337570524463,-0.893726913198842,
8.68099425934154));
#10618=CARTESIAN_POINT('Ctrl Pts',(1.13571087813116,-0.168674579522828,
8.71889923674692));
#10619=CARTESIAN_POINT('Ctrl Pts',(0.94899413688568,0.65068751575287,8.75688888882341));
#10620=CARTESIAN_POINT('Ctrl Pts',(0.369924963489578,1.04461917501135,8.78861243968945));
#10621=CARTESIAN_POINT('Ctrl Pts',(-0.163212573764178,1.06304769871494,
8.81403513535945));
#10622=CARTESIAN_POINT('Ctrl Pts',(-0.582898835599307,0.916898919717624,
8.83524177562921));
#10623=CARTESIAN_POINT('Ctrl Pts',(-0.938452485791775,0.570332830031077,
8.8585957898151));
#10624=CARTESIAN_POINT('Ctrl Pts',(-1.098449244479,0.0521610218923669,8.88410456256871));
#10625=CARTESIAN_POINT('Ctrl Pts',(-0.990747044809017,-0.479905179357058,
8.9096503715829));
#10626=CARTESIAN_POINT('Ctrl Pts',(-0.641456339423732,-0.89652388800662,
8.93522327648824));
#10627=CARTESIAN_POINT('Ctrl Pts',(-0.134922280861396,-1.09521608917999,
8.96083178186041));
#10628=CARTESIAN_POINT('Ctrl Pts',(0.360901232907297,-1.03317015380971,
8.98433058053565));
#10629=CARTESIAN_POINT('Ctrl Pts',(0.739743448699196,-0.794125607724712,
9.00571660323141));
#10630=CARTESIAN_POINT('Ctrl Pts',(1.06162643141654,-0.361743804765045,
9.03140126883326));
#10631=CARTESIAN_POINT('Ctrl Pts',(1.11648086851777,0.345841238273162,9.06354866838759));
#10632=CARTESIAN_POINT('Ctrl Pts',(0.671412092383133,0.901879124054754,
9.09573676847456));
#10633=CARTESIAN_POINT('Ctrl Pts',(0.160560298699368,1.07883883046449,9.12152345956742));
#10634=CARTESIAN_POINT('Ctrl Pts',(-0.31245850549709,1.06211512228001,9.14410225952631));
#10635=CARTESIAN_POINT('Ctrl Pts',(-0.797077087897755,0.794518382245735,
9.16992696032854));
#10636=CARTESIAN_POINT('Ctrl Pts',(-1.09856425898481,0.249118120983399,
9.19900933156918));
#10637=CARTESIAN_POINT('Ctrl Pts',(-1.06380000922336,-0.374144935055997,
9.22811991749506));
#10638=CARTESIAN_POINT('Ctrl Pts',(-0.769172046065886,-0.788482110834251,
9.25185920107736));
#10639=CARTESIAN_POINT('Ctrl Pts',(-0.367182194896042,-1.03416770199381,
9.27453758860991));
#10640=CARTESIAN_POINT('Ctrl Pts',(0.0395215134476794,-1.10612289271203,
9.29398716301566));
#10641=CARTESIAN_POINT('Ctrl Pts',(0.477622137462348,-0.988239329641883,
9.315608935922));
#10642=CARTESIAN_POINT('Ctrl Pts',(0.806060476953854,-0.746133466732723,
9.33508059295667));
#10643=CARTESIAN_POINT('Ctrl Pts',(1.02338097622177,-0.400209794823969,
9.35455900998878));
#10644=CARTESIAN_POINT('Ctrl Pts',(1.09301857284269,-0.0322005400116846,
9.37242337753565));
#10645=CARTESIAN_POINT('Ctrl Pts',(1.04557123688016,0.302448473621783,9.38867049786501));
#10646=CARTESIAN_POINT('Ctrl Pts',(0.880248597472728,0.673138628508302,
9.40817382201824));
#10647=CARTESIAN_POINT('Ctrl Pts',(0.490987821358575,1.0215162740493,9.43255931556892));
#10648=CARTESIAN_POINT('Ctrl Pts',(-0.128028731061003,1.12673431002624,
9.46184150098951));
#10649=CARTESIAN_POINT('Ctrl Pts',(-0.611115346897492,0.92634451080831,
9.48625316647187));
#10650=CARTESIAN_POINT('Ctrl Pts',(-0.890003906782786,0.630491031563606,
9.50579262818851));
#10651=CARTESIAN_POINT('Ctrl Pts',(-1.07718613810329,0.269493001893084,
9.52533614230101));
#10652=CARTESIAN_POINT('Ctrl Pts',(-1.10685316099274,-0.253206849806021,
9.549769143617));
#10653=CARTESIAN_POINT('Ctrl Pts',(-0.802665388553327,-0.80350029659764,
9.57910079014067));
#10654=CARTESIAN_POINT('Ctrl Pts',(-0.252382142420839,-1.10765434668513,
9.60844033627772));
#10655=CARTESIAN_POINT('Ctrl Pts',(0.375622844421776,-1.07241880015879,
9.6377872616149));
#10656=CARTESIAN_POINT('Ctrl Pts',(0.888675653575918,-0.708384464521095,
9.66713948562636));
#10657=CARTESIAN_POINT('Ctrl Pts',(1.12945283978432,-0.127110607216331,
9.69649562191789));
#10658=CARTESIAN_POINT('Ctrl Pts',(1.02406436855865,0.493221535835591,9.72585399659149));
#10659=CARTESIAN_POINT('Ctrl Pts',(0.604750564115747,0.962410167163729,
9.75521300373452));
#10660=CARTESIAN_POINT('Ctrl Pts',(0.00018168777481138,1.13659797379318,
9.78457113260792));
#10661=CARTESIAN_POINT('Ctrl Pts',(-0.604514012247553,0.962442862813792,
9.81392653168396));
#10662=CARTESIAN_POINT('Ctrl Pts',(-1.00788755091294,0.510743356018493,
9.84219098822073));
#10663=CARTESIAN_POINT('Ctrl Pts',(-1.12223084029966,-0.0555269185822364,
9.86936284287987));
#10664=CARTESIAN_POINT('Ctrl Pts',(-0.958681149169006,-0.584986935290896,
9.89544464218138));
#10665=CARTESIAN_POINT('Ctrl Pts',(-0.595072606804766,-0.939890399434298,
9.91934680514532));
#10666=CARTESIAN_POINT('Ctrl Pts',(-0.165261742340907,-1.08943840079317,
9.94106900696797));
#10667=CARTESIAN_POINT('Ctrl Pts',(0.381501891532602,-1.07053143388919,
9.96713134343117));
#10668=CARTESIAN_POINT('Ctrl Pts',(0.856595948124104,-0.748119235797807,
9.99318006438684));
#10669=CARTESIAN_POINT('Ctrl Pts',(1.07309034940253,-0.246007820424173,
10.0192184485331));
#10670=CARTESIAN_POINT('Ctrl Pts',(1.09532486422704,0.299243704641549,10.0452489336159));
#10671=CARTESIAN_POINT('Ctrl Pts',(0.737208771049273,0.921717292357175,
10.0777646557385));
#10672=CARTESIAN_POINT('Ctrl Pts',(-0.0875976639157576,1.17590238091633,
10.1167545687155));
#10673=CARTESIAN_POINT('Ctrl Pts',(-0.775414432101575,0.843148981901611,
10.1513791941553));
#10674=CARTESIAN_POINT('Ctrl Pts',(-1.08237439891738,0.276792097832271,
10.1816522621836));
#10675=CARTESIAN_POINT('Ctrl Pts',(-1.08223987573992,-0.273905699897673,
10.2075837109931));
#10676=CARTESIAN_POINT('Ctrl Pts',(-0.819021356744807,-0.757885892152692,
10.2334953587529));
#10677=CARTESIAN_POINT('Ctrl Pts',(-0.35659410762715,-1.05617411390235,
10.2593858505813));
#10678=CARTESIAN_POINT('Ctrl Pts',(0.191709377129806,-1.09707930859612,
10.2852567627067));
#10679=CARTESIAN_POINT('Ctrl Pts',(0.619305370577929,-0.903938602256031,
10.307333480538));
#10680=CARTESIAN_POINT('Ctrl Pts',(0.880476818061234,-0.627047684176173,
10.3256298718571));
#10681=CARTESIAN_POINT('Ctrl Pts',(1.0658885916031,-0.26934857845919,10.3449924871254));
#10682=CARTESIAN_POINT('Ctrl Pts',(1.09515715586536,0.247897726642305,10.3691745552382));
#10683=CARTESIAN_POINT('Ctrl Pts',(0.794434828137204,0.79164810257108,10.3981621507212));
#10684=CARTESIAN_POINT('Ctrl Pts',(0.2513627005957,1.09165703572537,10.4271160993126));
#10685=CARTESIAN_POINT('Ctrl Pts',(-0.367454430252698,1.05680897175568,
10.4560357085573));
#10686=CARTESIAN_POINT('Ctrl Pts',(-0.872209226186921,0.698502678542679,
10.4849194330614));
#10687=CARTESIAN_POINT('Ctrl Pts',(-1.10868326692617,0.127308218351685,
10.5137661629812));
#10688=CARTESIAN_POINT('Ctrl Pts',(-1.00514471501034,-0.48133956103109,
10.5425746368362));
#10689=CARTESIAN_POINT('Ctrl Pts',(-0.594223537283247,-0.940976300734034,
10.5713437045289));
#10690=CARTESIAN_POINT('Ctrl Pts',(-0.002580678613507,-1.11129495562103,
10.6000722203793));
#10691=CARTESIAN_POINT('Ctrl Pts',(0.588129815347979,-0.940979629269841,
10.6287590718095));
#10692=CARTESIAN_POINT('Ctrl Pts',(0.997070643975556,-0.483175565710426,
10.6574031830034));
#10693=CARTESIAN_POINT('Ctrl Pts',(1.09960229356506,0.121100802476138,10.6860035048011));
#10694=CARTESIAN_POINT('Ctrl Pts',(0.86528778983678,0.686415227285098,10.7145590265277));
#10695=CARTESIAN_POINT('Ctrl Pts',(0.366920420197264,1.03984587815201,10.7430687635858));
#10696=CARTESIAN_POINT('Ctrl Pts',(-0.242097189914162,1.0738946711142,10.7715317681828));
#10697=CARTESIAN_POINT('Ctrl Pts',(-0.774990713253418,0.779200373976015,
10.7999471270303));
#10698=CARTESIAN_POINT('Ctrl Pts',(-1.06891817459263,0.2470593867986,10.8283139593686));
#10699=CARTESIAN_POINT('Ctrl Pts',(-1.03474665817,-0.358829623525622,10.8566314075575));
#10700=CARTESIAN_POINT('Ctrl Pts',(-0.684094896882393,-0.85283074565291,
10.8848986782965));
#10701=CARTESIAN_POINT('Ctrl Pts',(-0.125405267425638,-1.0840777799931,
10.9131149316417));
#10702=CARTESIAN_POINT('Ctrl Pts',(0.469566204102857,-0.982999822886529,
10.9412795295327));
#10703=CARTESIAN_POINT('Ctrl Pts',(0.918640045850225,-0.581294038472193,
10.9693914839116));
#10704=CARTESIAN_POINT('Ctrl Pts',(1.02944056689496,-0.1965869628994,10.9880983243323));
#10705=CARTESIAN_POINT('Ctrl Pts',(1.02946655913226,-0.00351001149624692,
10.997442756416));
#10706=CARTESIAN_POINT('Ctrl Pts',(0.932816117174745,0.00257753706438406,
7.82155541886881));
#10707=CARTESIAN_POINT('Ctrl Pts',(0.932792537460822,0.177733635780523,
7.83003252737339));
#10708=CARTESIAN_POINT('Ctrl Pts',(0.832395790527212,0.526201721661573,
7.84697613681209));
#10709=CARTESIAN_POINT('Ctrl Pts',(0.425544200513314,0.890172337838447,
7.87244618255503));
#10710=CARTESIAN_POINT('Ctrl Pts',(-0.11336388666004,0.98167567131432,7.89795412018352));
#10711=CARTESIAN_POINT('Ctrl Pts',(-0.61933707944609,0.772243525278785,
7.92350765312756));
#10712=CARTESIAN_POINT('Ctrl Pts',(-0.936881339315919,0.324863039572081,
7.94910507894627));
#10713=CARTESIAN_POINT('Ctrl Pts',(-0.96782639358118,-0.223839618027314,
7.97474887367392));
#10714=CARTESIAN_POINT('Ctrl Pts',(-0.701621350606369,-0.705803746925262,
8.00043961028665));
#10715=CARTESIAN_POINT('Ctrl Pts',(-0.218907478333097,-0.972762223001147,
8.02617867435414));
#10716=CARTESIAN_POINT('Ctrl Pts',(0.332899340942218,-0.941930890565723,
8.0519670470666));
#10717=CARTESIAN_POINT('Ctrl Pts',(0.78460355937521,-0.62162490930732,8.07780583779769));
#10718=CARTESIAN_POINT('Ctrl Pts',(0.997079900383295,-0.109076731898229,
8.10369604591022));
#10719=CARTESIAN_POINT('Ctrl Pts',(0.904115937338599,0.439056301982027,
8.12963867407103));
#10720=CARTESIAN_POINT('Ctrl Pts',(0.533006028155458,0.854574243625169,
8.1556346512764));
#10721=CARTESIAN_POINT('Ctrl Pts',(-0.0033797306614811,1.00926211236485,
8.18168490546527));
#10722=CARTESIAN_POINT('Ctrl Pts',(-0.541040252974749,0.854578896037574,
8.2077902454942));
#10723=CARTESIAN_POINT('Ctrl Pts',(-0.900819615004692,0.452035261399126,
8.232982646847));
#10724=CARTESIAN_POINT('Ctrl Pts',(-0.986407683770965,0.0272443707704438,
8.25337195355103));
#10725=CARTESIAN_POINT('Ctrl Pts',(-0.937109814892794,-0.251094083734033,
8.26698515637403));
#10726=CARTESIAN_POINT('Ctrl Pts',(-0.880272398528943,-0.401369554301966,
8.27476997312653));
#10727=CARTESIAN_POINT('Ctrl Pts',(-0.767699859183187,-0.614677280654596,
8.28645287628459));
#10728=CARTESIAN_POINT('Ctrl Pts',(-0.50103538805602,-0.874994963856704,
8.30399768727805));
#10729=CARTESIAN_POINT('Ctrl Pts',(-0.0213267761989935,-1.01048232574384,
8.3274382097326));
#10730=CARTESIAN_POINT('Ctrl Pts',(0.464863835130203,-0.898942626339521,
8.35092523032543));
#10731=CARTESIAN_POINT('Ctrl Pts',(0.903709188564727,-0.513852403673233,
8.378381904535));
#10732=CARTESIAN_POINT('Ctrl Pts',(1.05988003651373,0.163448042572348,8.40983937592686));
#10733=CARTESIAN_POINT('Ctrl Pts',(0.710583436266589,0.766752724788841,
8.44139319618407));
#10734=CARTESIAN_POINT('Ctrl Pts',(0.1735498784337,1.0078575404005,8.46907468175037));
#10735=CARTESIAN_POINT('Ctrl Pts',(-0.329995702322566,0.970390012101335,
8.49285073236006));
#10736=CARTESIAN_POINT('Ctrl Pts',(-0.720223604553968,0.718362602848667,
8.51469007548597));
#10737=CARTESIAN_POINT('Ctrl Pts',(-0.941451908882603,0.365265796603737,
8.53458030754323));
#10738=CARTESIAN_POINT('Ctrl Pts',(-1.03626047645768,-0.127279523370467,
8.55848580751551));
#10739=CARTESIAN_POINT('Ctrl Pts',(-0.795928784219165,-0.74311800603862,
8.58843676936027));
#10740=CARTESIAN_POINT('Ctrl Pts',(-0.0776928783325622,-1.08960753239903,
8.62449067399998));
#10741=CARTESIAN_POINT('Ctrl Pts',(0.685958843373295,-0.854222896365132,
8.6606570762863));
#10742=CARTESIAN_POINT('Ctrl Pts',(1.08739997467006,-0.160417924516188,
8.6969363405203));
#10743=CARTESIAN_POINT('Ctrl Pts',(0.908689963674042,0.624433563761331,
8.73332847548848));
#10744=CARTESIAN_POINT('Ctrl Pts',(0.35355644738896,1.00221415934711,8.76374905337087));
#10745=CARTESIAN_POINT('Ctrl Pts',(-0.157958762417835,1.01991936283588,
8.788141995761));
#10746=CARTESIAN_POINT('Ctrl Pts',(-0.560829075860804,0.87964148645711,
8.80850060768873));
#10747=CARTESIAN_POINT('Ctrl Pts',(-0.902376151855375,0.546783264171767,
8.83093497234893));
#10748=CARTESIAN_POINT('Ctrl Pts',(-1.05620262261865,0.0487131824532962,
8.85545846822155));
#10749=CARTESIAN_POINT('Ctrl Pts',(-0.952659486533578,-0.46308305095605,
8.88003143979645));
#10750=CARTESIAN_POINT('Ctrl Pts',(-0.616438751614575,-0.864172093596548,
8.90465367965298));
#10751=CARTESIAN_POINT('Ctrl Pts',(-0.128491501662308,-1.05563283300167,
8.929324858834));
#10752=CARTESIAN_POINT('Ctrl Pts',(0.349568464277159,-0.995857144249034,
8.95198485171474));
#10753=CARTESIAN_POINT('Ctrl Pts',(0.715092597634469,-0.765243557764514,
8.97262009973951));
#10754=CARTESIAN_POINT('Ctrl Pts',(1.02585817273875,-0.347854923658281,
8.99741854820384));
#10755=CARTESIAN_POINT('Ctrl Pts',(1.07902066886242,0.335854720189213,9.02848390246269));
#10756=CARTESIAN_POINT('Ctrl Pts',(0.64850518863454,0.874001973235243,9.05963864033205));
#10757=CARTESIAN_POINT('Ctrl Pts',(0.153754709377709,1.04541750824584,9.08461452336056));
#10758=CARTESIAN_POINT('Ctrl Pts',(-0.304660404754024,1.02923830963297,
9.10649891467337));
#10759=CARTESIAN_POINT('Ctrl Pts',(-0.774772226567215,0.769734721067703,
9.13155302818068));
#10760=CARTESIAN_POINT('Ctrl Pts',(-1.06758176764164,0.240194096660453,
9.15979645527093));
#10761=CARTESIAN_POINT('Ctrl Pts',(-1.03388209497993,-0.365632688574458,
9.1880966422963));
#10762=CARTESIAN_POINT('Ctrl Pts',(-0.747236634374738,-0.768864123830532,
9.21120196811848));
#10763=CARTESIAN_POINT('Ctrl Pts',(-0.355793348154831,-1.0081210605673,
9.23328752841953));
#10764=CARTESIAN_POINT('Ctrl Pts',(0.0405271187519368,-1.0782861333172,
9.25224234259836));
#10765=CARTESIAN_POINT('Ctrl Pts',(0.467851885055523,-0.963334110221332,
9.27333469283053));
#10766=CARTESIAN_POINT('Ctrl Pts',(0.788437476668796,-0.727044639163456,
9.2923412041483));
#10767=CARTESIAN_POINT('Ctrl Pts',(1.0007528826234,-0.389147467838417,9.3113715890792));
#10768=CARTESIAN_POINT('Ctrl Pts',(1.06885322196228,-0.0293996181272015,
9.32883720111315));
#10769=CARTESIAN_POINT('Ctrl Pts',(1.02245490094734,0.297953905849491,9.34473160287988));
#10770=CARTESIAN_POINT('Ctrl Pts',(0.86066371709643,0.660768124405153,9.36382175120697));
#10771=CARTESIAN_POINT('Ctrl Pts',(0.479374090360282,1.00212138313223,9.38771687527452));
#10772=CARTESIAN_POINT('Ctrl Pts',(-0.127718095046861,1.10542227002233,
9.41643972739237));
#10773=CARTESIAN_POINT('Ctrl Pts',(-0.602123430277001,0.90873622757722,
9.4404161706225));
#10774=CARTESIAN_POINT('Ctrl Pts',(-0.876217908012786,0.617994917673252,
9.45962012033667));
#10775=CARTESIAN_POINT('Ctrl Pts',(-1.06029538877664,0.263022921439863,
9.47883959441989));
#10776=CARTESIAN_POINT('Ctrl Pts',(-1.08958045724843,-0.25145714410997,
9.50289353969035));
#10777=CARTESIAN_POINT('Ctrl Pts',(-0.789910095070733,-0.793793425585321,
9.53180255933616));
#10778=CARTESIAN_POINT('Ctrl Pts',(-0.247026510336,-1.09398288546205,9.56075524452346));
#10779=CARTESIAN_POINT('Ctrl Pts',(0.373354429623973,-1.05928378029671,
9.58975007442778));
#10780=CARTESIAN_POINT('Ctrl Pts',(0.880858555852544,-0.699321360637946,
9.61878586997401));
#10781=CARTESIAN_POINT('Ctrl Pts',(1.11939651791946,-0.123739308088276,
9.64786125750938));
#10782=CARTESIAN_POINT('Ctrl Pts',(1.01501061604786,0.491341759208262,9.67697489434579));
#10783=CARTESIAN_POINT('Ctrl Pts',(0.598822393739831,0.957195198398869,
9.70612540386286));
#10784=CARTESIAN_POINT('Ctrl Pts',(-0.00207634075492403,1.13043680813235,
9.73531134564448));
#10785=CARTESIAN_POINT('Ctrl Pts',(-0.603912123248523,0.957215276033718,
9.76453137942698));
#10786=CARTESIAN_POINT('Ctrl Pts',(-1.00594389361736,0.507177516237079,
9.79270042150575));
#10787=CARTESIAN_POINT('Ctrl Pts',(-1.12009446569155,-0.0577553123758345,
9.81981342467293));
#10788=CARTESIAN_POINT('Ctrl Pts',(-0.956831265840032,-0.586568536389845,
9.8458643888034));
#10789=CARTESIAN_POINT('Ctrl Pts',(-0.593322824365002,-0.941465991223857,
9.8697649885894));
#10790=CARTESIAN_POINT('Ctrl Pts',(-0.163152777889603,-1.09117482218559,
9.89150891502364));
#10791=CARTESIAN_POINT('Ctrl Pts',(0.384507054175381,-1.07229194200837,
9.91761601463539));
#10792=CARTESIAN_POINT('Ctrl Pts',(0.861095137732964,-0.749070261446909,
9.94374661664145));
#10793=CARTESIAN_POINT('Ctrl Pts',(1.07855069686503,-0.24487939037421,9.96989644300623));
#10794=CARTESIAN_POINT('Ctrl Pts',(1.10093949076505,0.303072931485129,9.9960586104448));
#10795=CARTESIAN_POINT('Ctrl Pts',(0.74077341907722,0.929563584544601,10.0287865624482));
#10796=CARTESIAN_POINT('Ctrl Pts',(-0.0904825710551195,1.18602420370029,
10.0680912360091));
#10797=CARTESIAN_POINT('Ctrl Pts',(-0.785003918826264,0.850284549087302,
10.1030550955328));
#10798=CARTESIAN_POINT('Ctrl Pts',(-1.0954014372141,0.277765624320416,10.1336635590215));
#10799=CARTESIAN_POINT('Ctrl Pts',(-1.09534339945125,-0.279543559457623,
10.1599082341136));
#10800=CARTESIAN_POINT('Ctrl Pts',(-0.828733022228398,-0.769900103510982,
10.1861618892393));
#10801=CARTESIAN_POINT('Ctrl Pts',(-0.359774220131184,-1.07248984309679,
10.212423484559));
#10802=CARTESIAN_POINT('Ctrl Pts',(0.196885914186667,-1.11409518777613,
10.2386900633088));
#10803=CARTESIAN_POINT('Ctrl Pts',(0.631515451668511,-0.917851149722072,
10.2611320934233));
#10804=CARTESIAN_POINT('Ctrl Pts',(0.897179887249006,-0.636222443941654,
10.2797433547922));
#10805=CARTESIAN_POINT('Ctrl Pts',(1.0858961146808,-0.272190094723938,10.2994507035648));
#10806=CARTESIAN_POINT('Ctrl Pts',(1.11580087037807,0.254712868751099,10.3240884429413));
#10807=CARTESIAN_POINT('Ctrl Pts',(0.809208599810454,0.809296967356682,
10.353654139103));
#10808=CARTESIAN_POINT('Ctrl Pts',(0.254788423957568,1.11569881651034,10.383219698794));
#10809=CARTESIAN_POINT('Ctrl Pts',(-0.377734849108055,1.08018316957416,
10.4127829355374));
#10810=CARTESIAN_POINT('Ctrl Pts',(-0.894297933370396,0.713620441102003,
10.4423423586806));
#10811=CARTESIAN_POINT('Ctrl Pts',(-1.13663484410025,0.128525956779319,
10.4718961659386));
#10812=CARTESIAN_POINT('Ctrl Pts',(-1.03055159767899,-0.495666761823774,
10.5014426885714));
#10813=CARTESIAN_POINT('Ctrl Pts',(-0.608768055200784,-0.967598798699277,
10.5309801966361));
#10814=CARTESIAN_POINT('Ctrl Pts',(-0.000768715985731294,-1.14272525987886,
10.5605070077873));
#10815=CARTESIAN_POINT('Ctrl Pts',(0.606953484275095,-0.967602860308774,
10.5900214114748));
#10816=CARTESIAN_POINT('Ctrl Pts',(1.02815040642715,-0.496217147831501,
10.6195217311575));
#10817=CARTESIAN_POINT('Ctrl Pts',(1.13393293838566,0.126674177284328,10.6490062827704));
#10818=CARTESIAN_POINT('Ctrl Pts',(0.892240327216091,0.710023030082336,
10.6784734108048));
#10819=CARTESIAN_POINT('Ctrl Pts',(0.37756151121538,1.0751290249391,10.7079214511558));
#10820=CARTESIAN_POINT('Ctrl Pts',(-0.252037482971,1.11041475463464,10.7373487814911));
#10821=CARTESIAN_POINT('Ctrl Pts',(-0.803490717852888,0.805552343975863,
10.7667537501932));
#10822=CARTESIAN_POINT('Ctrl Pts',(-1.10797664005012,0.254464265888738,
10.796134828178));
#10823=CARTESIAN_POINT('Ctrl Pts',(-1.07263280292657,-0.373598325782701,
10.8254902498732));
#10824=CARTESIAN_POINT('Ctrl Pts',(-0.708901590711751,-0.88615095694047,
10.8548188612348));
#10825=CARTESIAN_POINT('Ctrl Pts',(-0.128820897427331,-1.12633619172926,
10.8841182058041));
#10826=CARTESIAN_POINT('Ctrl Pts',(0.489474256939415,-1.02135047902734,
10.9133888202114));
#10827=CARTESIAN_POINT('Ctrl Pts',(0.956556872453774,-0.603666350937339,
10.9426246469134));
#10828=CARTESIAN_POINT('Ctrl Pts',(1.07193781572403,-0.203201562396062,
10.9621000587781));
#10829=CARTESIAN_POINT('Ctrl Pts',(1.07196486456811,-0.00227586712733216,
10.9718243500499));
#10830=CARTESIAN_POINT('Ctrl Pts',(0.916386464361943,-0.00093309831050743,
7.8940473292219));
#10831=CARTESIAN_POINT('Ctrl Pts',(0.916363306673161,0.171088090561208,
7.90237271608449));
#10832=CARTESIAN_POINT('Ctrl Pts',(0.817709848796121,0.513018539755372,
7.91900290782367));
#10833=CARTESIAN_POINT('Ctrl Pts',(0.419193318564387,0.869300720967443,
7.94394562555401));
#10834=CARTESIAN_POINT('Ctrl Pts',(-0.107459845420563,0.958570197177955,
7.96887498479583));
#10835=CARTESIAN_POINT('Ctrl Pts',(-0.600815190480234,0.754199282249767,
7.99379660366029));
#10836=CARTESIAN_POINT('Ctrl Pts',(-0.90972475540008,0.318735876207034,
8.01871040893382));
#10837=CARTESIAN_POINT('Ctrl Pts',(-0.939634168320183,-0.214178713135979,
8.04361889595454));
#10838=CARTESIAN_POINT('Ctrl Pts',(-0.681480351317133,-0.681266235779645,
8.06852342334305));
#10839=CARTESIAN_POINT('Ctrl Pts',(-0.214442030770815,-0.939390273067314,
8.0934258663209));
#10840=CARTESIAN_POINT('Ctrl Pts',(0.318328618727776,-0.909478985290061,
8.11832788264496));
#10841=CARTESIAN_POINT('Ctrl Pts',(0.753548017202942,-0.600689198431121,
8.14323122154075));
#10842=CARTESIAN_POINT('Ctrl Pts',(0.957798608325141,-0.107620541089113,
8.16813759793459));
#10843=CARTESIAN_POINT('Ctrl Pts',(0.868405979460084,0.418636976277688,
8.19304874272053));
#10844=CARTESIAN_POINT('Ctrl Pts',(0.512629065363514,0.816784590937834,
8.21796638811051));
#10845=CARTESIAN_POINT('Ctrl Pts',(-0.000585672768811046,0.964652867330779,
8.24289223431723));
#10846=CARTESIAN_POINT('Ctrl Pts',(-0.514067682434154,0.816790328676347,
8.26782807268141));
#10847=CARTESIAN_POINT('Ctrl Pts',(-0.857028397869778,0.432886852605677,
8.29185151518157));
#10848=CARTESIAN_POINT('Ctrl Pts',(-0.938441693019448,0.0284593721668554,
8.31126498760023));
#10849=CARTESIAN_POINT('Ctrl Pts',(-0.891549619244174,-0.236233682506208,
8.32421168378805));
#10850=CARTESIAN_POINT('Ctrl Pts',(-0.837526115658479,-0.379066140937872,
8.33161111168448));
#10851=CARTESIAN_POINT('Ctrl Pts',(-0.730561974805884,-0.581738446354059,
8.34271189331387));
#10852=CARTESIAN_POINT('Ctrl Pts',(-0.477352425520727,-0.828842529403336,
8.35937075304238));
#10853=CARTESIAN_POINT('Ctrl Pts',(-0.0225330382004105,-0.957209024892203,
8.38159488569873));
#10854=CARTESIAN_POINT('Ctrl Pts',(0.437788178382466,-0.851537961861344,
8.40383465770076));
#10855=CARTESIAN_POINT('Ctrl Pts',(0.852715694662685,-0.487307649407337,
8.42980009152249));
#10856=CARTESIAN_POINT('Ctrl Pts',(0.999965381191419,0.152241057725198,
8.45950561391401));
#10857=CARTESIAN_POINT('Ctrl Pts',(0.670567292988393,0.720763590006567,
8.48924952521388));
#10858=CARTESIAN_POINT('Ctrl Pts',(0.165104121582195,0.947610229347272,
8.51530399445417));
#10859=CARTESIAN_POINT('Ctrl Pts',(-0.308304372080754,0.912327630374344,
8.53765800829594));
#10860=CARTESIAN_POINT('Ctrl Pts',(-0.67477683344297,0.675573610699686,
8.55817118909699));
#10861=CARTESIAN_POINT('Ctrl Pts',(-0.882350277706418,0.34422728689363,
8.57683651179162));
#10862=CARTESIAN_POINT('Ctrl Pts',(-0.971219773321951,-0.117642462843675,
8.59925338393781));
#10863=CARTESIAN_POINT('Ctrl Pts',(-0.745953604143611,-0.694472541682851,
8.62731233232217));
#10864=CARTESIAN_POINT('Ctrl Pts',(-0.0739633240472909,-1.01845581262107,
8.66104313406658));
#10865=CARTESIAN_POINT('Ctrl Pts',(0.63952747451705,-0.798369631564053,
8.69483872901917));
#10866=CARTESIAN_POINT('Ctrl Pts',(1.01408422655149,-0.150734124008621,
8.72870212818689));
#10867=CARTESIAN_POINT('Ctrl Pts',(0.847322126498796,0.58103611525318,8.76263640124927));
#10868=CARTESIAN_POINT('Ctrl Pts',(0.330121026915543,0.932886604391724,
8.79097752783638));
#10869=CARTESIAN_POINT('Ctrl Pts',(-0.146093769553075,0.949351984337242,
8.81368784917009));
#10870=CARTESIAN_POINT('Ctrl Pts',(-0.521021746649022,0.818789575072917,
8.83263515205418));
#10871=CARTESIAN_POINT('Ctrl Pts',(-0.838737700087821,0.509122269324307,
8.85350597952678));
#10872=CARTESIAN_POINT('Ctrl Pts',(-0.981754612397829,0.0459670008233027,
8.87631102562348));
#10873=CARTESIAN_POINT('Ctrl Pts',(-0.885491145123779,-0.429752885191932,
8.89915236426619));
#10874=CARTESIAN_POINT('Ctrl Pts',(-0.573052273480284,-0.802442728830194,
8.9220328462699));
#10875=CARTESIAN_POINT('Ctrl Pts',(-0.11977334499688,-0.980285495206635,
8.94495124212259));
#10876=CARTESIAN_POINT('Ctrl Pts',(0.324211584585207,-0.924759915662738,
8.96599677624005));
#10877=CARTESIAN_POINT('Ctrl Pts',(0.663619579763974,-0.710620166507527,
8.98515810751412));
#10878=CARTESIAN_POINT('Ctrl Pts',(0.952143685172452,-0.323095904167005,
9.00818238284112));
#10879=CARTESIAN_POINT('Ctrl Pts',(1.00147844946261,0.311593665089388,9.03702060642391));
#10880=CARTESIAN_POINT('Ctrl Pts',(0.601866958953658,0.811110161437164,
9.06593988482292));
#10881=CARTESIAN_POINT('Ctrl Pts',(0.142635782304362,0.970222188044987,
9.08912285438075));
#10882=CARTESIAN_POINT('Ctrl Pts',(-0.282880216341775,0.955206494432585,
9.10943681406231));
#10883=CARTESIAN_POINT('Ctrl Pts',(-0.719285418358596,0.714319703027661,
9.13269449197724));
#10884=CARTESIAN_POINT('Ctrl Pts',(-0.991145548172263,0.222695996518761,
9.1589160433785));
#10885=CARTESIAN_POINT('Ctrl Pts',(-0.9598723234409,-0.33986314694992,9.18519504623541));
#10886=CARTESIAN_POINT('Ctrl Pts',(-0.693651734536496,-0.714395587302459,
9.20665515597952));
#10887=CARTESIAN_POINT('Ctrl Pts',(-0.33000558647281,-0.936668388183705,
9.22717248577931));
#10888=CARTESIAN_POINT('Ctrl Pts',(0.0382488951801815,-1.00187881354344,
9.24478504858718));
#10889=CARTESIAN_POINT('Ctrl Pts',(0.435428514213863,-0.895048693578503,
9.26438909498248));
#10890=CARTESIAN_POINT('Ctrl Pts',(0.733481601998805,-0.67537933957951,
9.28205927527633));
#10891=CARTESIAN_POINT('Ctrl Pts',(0.930935942815539,-0.361155740600938,
9.29975646442145));
#10892=CARTESIAN_POINT('Ctrl Pts',(0.994297368624369,-0.0265033935802915,
9.31600357587152));
#10893=CARTESIAN_POINT('Ctrl Pts',(0.951128789628544,0.278106881586742,
9.33079344806764));
#10894=CARTESIAN_POINT('Ctrl Pts',(0.800547029468414,0.615803482990443,
9.34856170352529));
#10895=CARTESIAN_POINT('Ctrl Pts',(0.445541906176031,0.933679329429137,
9.37081057426095));
#10896=CARTESIAN_POINT('Ctrl Pts',(-0.120075741503171,1.02997680518912,
9.39757104683856));
#10897=CARTESIAN_POINT('Ctrl Pts',(-0.562380172430049,0.846648767025865,
9.41992332291532));
#10898=CARTESIAN_POINT('Ctrl Pts',(-0.818063047449599,0.575452122500431,
9.43783641698758));
#10899=CARTESIAN_POINT('Ctrl Pts',(-0.989839448666035,0.24422322307351,
9.45577041101522));
#10900=CARTESIAN_POINT('Ctrl Pts',(-1.01723457777004,-0.236110259423285,
9.47822706382322));
#10901=CARTESIAN_POINT('Ctrl Pts',(-0.737289662342792,-0.742891434307192,
9.50523810407958));
#10902=CARTESIAN_POINT('Ctrl Pts',(-0.229642005372076,-1.02367828901602,
9.53231229849314));
#10903=CARTESIAN_POINT('Ctrl Pts',(0.351027390123253,-0.991276097967053,
9.559449788874));
#10904=CARTESIAN_POINT('Ctrl Pts',(0.826527285725571,-0.654110782122341,
9.58665063199169));
#10905=CARTESIAN_POINT('Ctrl Pts',(1.05029403858789,-0.11438813617086,9.61391485224451));
#10906=CARTESIAN_POINT('Ctrl Pts',(0.952393012397771,0.463003902808121,
9.64124242605231));
#10907=CARTESIAN_POINT('Ctrl Pts',(0.561373841868419,0.900822151844062,
9.66863326977439));
#10908=CARTESIAN_POINT('Ctrl Pts',(-0.00387276695331408,1.0638843291464,
9.69608728519562));
#10909=CARTESIAN_POINT('Ctrl Pts',(-0.570695551262971,0.900845596732101,
9.723604249157));
#10910=CARTESIAN_POINT('Ctrl Pts',(-0.949833801943534,0.476579569449792,
9.75016258055998));
#10911=CARTESIAN_POINT('Ctrl Pts',(-1.05766462295084,-0.0566720978017236,
9.77575398707171));
#10912=CARTESIAN_POINT('Ctrl Pts',(-0.903446650287503,-0.556425680500337,
9.80037141569279));
#10913=CARTESIAN_POINT('Ctrl Pts',(-0.55959314493252,-0.892235666458625,
9.82298223779303));
#10914=CARTESIAN_POINT('Ctrl Pts',(-0.152220323052832,-1.03404623235443,
9.84357273851314));
#10915=CARTESIAN_POINT('Ctrl Pts',(0.366883172029728,-1.01619539695405,
9.86831820213365));
#10916=CARTESIAN_POINT('Ctrl Pts',(0.819317002651662,-0.709565750262104,
9.89311712889566));
#10917=CARTESIAN_POINT('Ctrl Pts',(1.02605541148877,-0.230354394394416,
9.91797028804756));
#10918=CARTESIAN_POINT('Ctrl Pts',(1.04740076386437,0.290941337297571,9.94285927862722));
#10919=CARTESIAN_POINT('Ctrl Pts',(0.704487085949529,0.887918159178826,
9.97403534857104));
#10920=CARTESIAN_POINT('Ctrl Pts',(-0.0889329641953167,1.13305086915798,
10.0115520936496));
#10921=CARTESIAN_POINT('Ctrl Pts',(-0.753378607817973,0.812154603631431,
10.0449913261173));
#10922=CARTESIAN_POINT('Ctrl Pts',(-1.0509061430146,0.2636345725963,10.0743168693977));
#10923=CARTESIAN_POINT('Ctrl Pts',(-1.05093739784869,-0.271120657455177,
10.0994981767143));
#10924=CARTESIAN_POINT('Ctrl Pts',(-0.794853058550813,-0.742337793921308,
10.1247231042996));
#10925=CARTESIAN_POINT('Ctrl Pts',(-0.343652569312813,-1.03358848122898,
10.1499909616499));
#10926=CARTESIAN_POINT('Ctrl Pts',(0.192775959815744,-1.07377917166597,
10.1753023818525));
#10927=CARTESIAN_POINT('Ctrl Pts',(0.612246298230531,-0.884472212478353,
10.1969571970733));
#10928=CARTESIAN_POINT('Ctrl Pts',(0.868951664888123,-0.612372118526421,
10.2149387020014));
#10929=CARTESIAN_POINT('Ctrl Pts',(1.05146362716697,-0.260359176846704,
10.2339952372064));
#10930=CARTESIAN_POINT('Ctrl Pts',(1.08053751648403,0.249785530435256,10.2578467531362));
#10931=CARTESIAN_POINT('Ctrl Pts',(0.783308174548958,0.787746446449566,
10.2865196367573));
#10932=CARTESIAN_POINT('Ctrl Pts',(0.244719009240793,1.08556755291199,10.3152415913622));
#10933=CARTESIAN_POINT('Ctrl Pts',(-0.370909273962754,1.05115342677162,
10.3440118820671));
#10934=CARTESIAN_POINT('Ctrl Pts',(-0.874646110508742,0.693881654635859,
10.3728291813908));
#10935=CARTESIAN_POINT('Ctrl Pts',(-1.11148911187944,0.122460707441426,
10.4016923877211));
#10936=CARTESIAN_POINT('Ctrl Pts',(-1.00784436408095,-0.488329418075964,
10.4306002515908));
#10937=CARTESIAN_POINT('Ctrl Pts',(-0.594508503032201,-0.95104895241576,
10.4595515415207));
#10938=CARTESIAN_POINT('Ctrl Pts',(0.00252468810929164,-1.12318404866533,
10.4885449844876));
#10939=CARTESIAN_POINT('Ctrl Pts',(0.600466974195298,-0.951048000094383,
10.517579269984));
#10940=CARTESIAN_POINT('Ctrl Pts',(1.0157379397141,-0.486537895502348,10.5466530692494));
#10941=CARTESIAN_POINT('Ctrl Pts',(1.12035505762534,0.128518294750485,10.5757650148325));
#10942=CARTESIAN_POINT('Ctrl Pts',(0.881400098068042,0.705686601319807,
10.6049137245664));
#10943=CARTESIAN_POINT('Ctrl Pts',(0.371376215689227,1.06769185969133,10.6340977709503));
#10944=CARTESIAN_POINT('Ctrl Pts',(-0.253801011916156,1.10289557553796,
10.66331572853));
#10945=CARTESIAN_POINT('Ctrl Pts',(-0.802494827547404,0.799749660182247,
10.6925660997033));
#10946=CARTESIAN_POINT('Ctrl Pts',(-1.1061282469781,0.250555575979397,10.7218474788459));
#10947=CARTESIAN_POINT('Ctrl Pts',(-1.07100530702942,-0.376623977361633,
10.7511581664581));
#10948=CARTESIAN_POINT('Ctrl Pts',(-0.707253391080627,-0.88950243387736,
10.7804970768219));
#10949=CARTESIAN_POINT('Ctrl Pts',(-0.125893311798114,-1.13040111480947,
10.8098616956024));
#10950=CARTESIAN_POINT('Ctrl Pts',(0.495010447492726,-1.02512577517357,
10.8392526661857));
#10951=CARTESIAN_POINT('Ctrl Pts',(0.96503436836903,-0.605029576661258,
10.8686635500669));
#10952=CARTESIAN_POINT('Ctrl Pts',(1.08139545050083,-0.201364018273147,
10.8882928173859));
#10953=CARTESIAN_POINT('Ctrl Pts',(1.08142273213372,0.00129089154989864,
10.8981007982325));
#10954=CARTESIAN_POINT('Ctrl Pts',(0.962718053183473,-0.00374989906965716,
7.95237763337882));
#10955=CARTESIAN_POINT('Ctrl Pts',(0.962693741742924,0.176841650701835,
7.96111780385329));
#10956=CARTESIAN_POINT('Ctrl Pts',(0.859087970836183,0.535837040265186,
7.97857651794297));
#10957=CARTESIAN_POINT('Ctrl Pts',(0.44139204471531,0.909067672566069,8.00471126618545));
#10958=CARTESIAN_POINT('Ctrl Pts',(-0.10957037240375,1.00234938185105,8.03078957638873));
#10959=CARTESIAN_POINT('Ctrl Pts',(-0.624736766215092,0.788788067770214,
8.05681339506897));
#10960=CARTESIAN_POINT('Ctrl Pts',(-0.946645438372464,0.334753964295622,
8.08278312833397));
#10961=CARTESIAN_POINT('Ctrl Pts',(-0.977622131806228,-0.219795110452919,
8.10869993425576));
#10962=CARTESIAN_POINT('Ctrl Pts',(-0.709358577384567,-0.704866328363871,
8.1345646888734));
#10963=CARTESIAN_POINT('Ctrl Pts',(-0.225106799315938,-0.972333316118095,
8.16037844801135));
#10964=CARTESIAN_POINT('Ctrl Pts',(0.326150581648902,-0.94123300043997,
8.18614224392964));
#10965=CARTESIAN_POINT('Ctrl Pts',(0.775513506064428,-0.622221923030926,
8.21185716800189));
#10966=CARTESIAN_POINT('Ctrl Pts',(0.98588437082731,-0.113978011641057,
8.23752433345641));
#10967=CARTESIAN_POINT('Ctrl Pts',(0.893783701493479,0.427300464910859,
8.26314490422908));
#10968=CARTESIAN_POINT('Ctrl Pts',(0.528462068175506,0.835896897170472,
8.2887200485398));
#10969=CARTESIAN_POINT('Ctrl Pts',(0.00268624907551326,0.987222480008646,
8.31425101187734));
#10970=CARTESIAN_POINT('Ctrl Pts',(-0.522182866084098,0.835917649550696,
8.33973897090827));
#10971=CARTESIAN_POINT('Ctrl Pts',(-0.87192408794217,0.444190331151998,
8.36424287105709));
#10972=CARTESIAN_POINT('Ctrl Pts',(-0.954708318592613,0.0324397670437707,
8.3840047340831));
#10973=CARTESIAN_POINT('Ctrl Pts',(-0.9070179840126,-0.236658638349185,
8.39716640171874));
#10974=CARTESIAN_POINT('Ctrl Pts',(-0.852130113915824,-0.38176994593457,
8.40468374381179));
#10975=CARTESIAN_POINT('Ctrl Pts',(-0.74350765580059,-0.587578812177685,
8.41595591900598));
#10976=CARTESIAN_POINT('Ctrl Pts',(-0.486647878371642,-0.838127844696909,
8.43284869457147));
#10977=CARTESIAN_POINT('Ctrl Pts',(-0.0261984492433358,-0.967968322662697,
8.45534493147975));
#10978=CARTESIAN_POINT('Ctrl Pts',(0.438852361093423,-0.861090302172016,
8.47781287489012));
#10979=CARTESIAN_POINT('Ctrl Pts',(0.857189010370208,-0.493690220081531,
8.50399399075845));
#10980=CARTESIAN_POINT('Ctrl Pts',(1.00495380425253,0.149738205456235,8.53387052514169));
#10981=CARTESIAN_POINT('Ctrl Pts',(0.67426857107042,0.719767262233913,8.56369821016954));
#10982=CARTESIAN_POINT('Ctrl Pts',(0.168456706986281,0.946614776845862,
8.58976630720376));
#10983=CARTESIAN_POINT('Ctrl Pts',(-0.304308025339452,0.91126669792293,
8.61208912631691));
#10984=CARTESIAN_POINT('Ctrl Pts',(-0.669501390402897,0.675208297254384,
8.63253180589755));
#10985=CARTESIAN_POINT('Ctrl Pts',(-0.875992946329232,0.345495322089341,
8.65110259959686));
#10986=CARTESIAN_POINT('Ctrl Pts',(-0.964223900143266,-0.113431902350383,
8.67337382774449));
#10987=CARTESIAN_POINT('Ctrl Pts',(-0.740596150234679,-0.685160402045384,
8.70118563330055));
#10988=CARTESIAN_POINT('Ctrl Pts',(-0.0761424558024043,-1.00505324721318,
8.73452517400358));
#10989=CARTESIAN_POINT('Ctrl Pts',(0.627005912154053,-0.787736452578971,
8.76783232144636));
#10990=CARTESIAN_POINT('Ctrl Pts',(0.994812400535726,-0.150994958894705,
8.80111127518668));
#10991=CARTESIAN_POINT('Ctrl Pts',(0.830981358300232,0.566120360011879,
8.8343664264926));
#10992=CARTESIAN_POINT('Ctrl Pts',(0.325333743617495,0.909742405641226,
8.86206095120001));
#10993=CARTESIAN_POINT('Ctrl Pts',(-0.139139429575983,0.925737554743745,
8.88421060397605));
#10994=CARTESIAN_POINT('Ctrl Pts',(-0.504321857670482,0.798522533185246,
8.90266440172502));
#10995=CARTESIAN_POINT('Ctrl Pts',(-0.813223734583826,0.497308829081565,
8.92295891595097));
#10996=CARTESIAN_POINT('Ctrl Pts',(-0.951958679300059,0.0476855097530266,
8.94509334884795));
#10997=CARTESIAN_POINT('Ctrl Pts',(-0.858568536947436,-0.413287554490503,
8.9672269803888));
#10998=CARTESIAN_POINT('Ctrl Pts',(-0.556269061692827,-0.773731542124292,
8.98935651187958));
#10999=CARTESIAN_POINT('Ctrl Pts',(-0.118502160687732,-0.945376823498998,
9.01148772025747));
#11000=CARTESIAN_POINT('Ctrl Pts',(0.309493444328896,-0.891756529896018,
9.03177362093023));
#11001=CARTESIAN_POINT('Ctrl Pts',(0.636192413112547,-0.685585808620992,
9.05021771711067));
#11002=CARTESIAN_POINT('Ctrl Pts',(0.913553474295901,-0.312947881864283,
9.07235265309009));
#11003=CARTESIAN_POINT('Ctrl Pts',(0.960631698996472,0.296194052975052,
9.10002751178583));
#11004=CARTESIAN_POINT('Ctrl Pts',(0.577840333647451,0.774226230638954,
9.12770811478922));
#11005=CARTESIAN_POINT('Ctrl Pts',(0.138921963035328,0.926247468472041,
9.14986447621748));
#11006=CARTESIAN_POINT('Ctrl Pts',(-0.267314239023255,0.911868754744674,
9.16925630150695));
#11007=CARTESIAN_POINT('Ctrl Pts',(-0.683294438003391,0.682129412884273,
9.19142590162011));
#11008=CARTESIAN_POINT('Ctrl Pts',(-0.941938680245144,0.214161666280006,
9.21638016709812));
#11009=CARTESIAN_POINT('Ctrl Pts',(-0.912098799441386,-0.320403545601203,
9.24134958755738));
#11010=CARTESIAN_POINT('Ctrl Pts',(-0.659446939725027,-0.675689901682901,
9.2617076691118));
#11011=CARTESIAN_POINT('Ctrl Pts',(-0.314783201133364,-0.886337451361902,
9.28115257773485));
#11012=CARTESIAN_POINT('Ctrl Pts',(0.0339048682581715,-0.948027262613349,
9.29782815531288));
#11013=CARTESIAN_POINT('Ctrl Pts',(0.409525764171749,-0.846956944511177,
9.3163673731042));
#11014=CARTESIAN_POINT('Ctrl Pts',(0.691138366917057,-0.639370288018321,
9.33306328330105));
#11015=CARTESIAN_POINT('Ctrl Pts',(0.87750645881461,-0.342726650725962,
9.34976804539523));
#11016=CARTESIAN_POINT('Ctrl Pts',(0.937239721660506,-0.0270902356967322,
9.36509083849118));
#11017=CARTESIAN_POINT('Ctrl Pts',(0.896541377625576,0.259988256337935,
9.37902894066585));
#11018=CARTESIAN_POINT('Ctrl Pts',(0.754698132227089,0.578045031261971,
9.39576347782597));
#11019=CARTESIAN_POINT('Ctrl Pts',(0.420607969490248,0.877087830349221,
9.41669599586192));
#11020=CARTESIAN_POINT('Ctrl Pts',(-0.110985791513677,0.96749605599269,
9.44184448602026));
#11021=CARTESIAN_POINT('Ctrl Pts',(-0.526156759994638,0.795331969305767,
9.46282505153596));
#11022=CARTESIAN_POINT('Ctrl Pts',(-0.765969009939309,0.540947935087001,
9.47962659419499));
#11023=CARTESIAN_POINT('Ctrl Pts',(-0.926993499156135,0.230420411283913,
9.49643868360314));
#11024=CARTESIAN_POINT('Ctrl Pts',(-0.952589676219305,-0.219519434718937,
9.51747248884386));
#11025=CARTESIAN_POINT('Ctrl Pts',(-0.690553452001334,-0.69372499155175,
9.54274789258842));
#11026=CARTESIAN_POINT('Ctrl Pts',(-0.215911709650212,-0.956173277204949,
9.56805844086952));
#11027=CARTESIAN_POINT('Ctrl Pts',(0.326482153616986,-0.925839193894392,
9.59340601342297));
#11028=CARTESIAN_POINT('Ctrl Pts',(0.770238105376938,-0.611104726507316,
9.61879177600974));
#11029=CARTESIAN_POINT('Ctrl Pts',(0.978868207415932,-0.107737371893569,
9.64421717352356));
#11030=CARTESIAN_POINT('Ctrl Pts',(0.887577227206843,0.430343959694922,
9.66968349904293));
#11031=CARTESIAN_POINT('Ctrl Pts',(0.523376342408703,0.838059053917545,
9.6951920503197));
#11032=CARTESIAN_POINT('Ctrl Pts',(-0.00274426362498771,0.989786805195399,
9.72074411643293));
#11033=CARTESIAN_POINT('Ctrl Pts',(-0.530020135210238,0.838080337149508,
9.7463408384755));
#11034=CARTESIAN_POINT('Ctrl Pts',(-0.882514473551932,0.443575823263503,
9.77103386810706));
#11035=CARTESIAN_POINT('Ctrl Pts',(-0.982710426754106,-0.0520415125974364,
9.79481815229705));
#11036=CARTESIAN_POINT('Ctrl Pts',(-0.839404992399888,-0.516361307665272,
9.81769006840781));
#11037=CARTESIAN_POINT('Ctrl Pts',(-0.520010572161815,-0.82826298112752,
9.83869155958704));
#11038=CARTESIAN_POINT('Ctrl Pts',(-0.141709529917495,-0.959945613344496,
9.85781211466694));
#11039=CARTESIAN_POINT('Ctrl Pts',(0.34027152731852,-0.943361696850372,
9.88078772261496));
#11040=CARTESIAN_POINT('Ctrl Pts',(0.7602508065088,-0.658700704986937,9.90380787473997));
#11041=CARTESIAN_POINT('Ctrl Pts',(0.952135045606276,-0.213907148975505,
9.92687574131966));
#11042=CARTESIAN_POINT('Ctrl Pts',(0.971942351738693,0.269920095428384,
9.94997564071361));
#11043=CARTESIAN_POINT('Ctrl Pts',(0.653688535130702,0.82395147603505,9.9789087386129));
#11044=CARTESIAN_POINT('Ctrl Pts',(-0.0826775166361059,1.05146637821754,
10.0137277686201));
#11045=CARTESIAN_POINT('Ctrl Pts',(-0.699434812986587,0.753622187593778,
10.0447664048801));
#11046=CARTESIAN_POINT('Ctrl Pts',(-0.975666081398681,0.244387937000841,
10.0719919503651));
#11047=CARTESIAN_POINT('Ctrl Pts',(-0.975707195393647,-0.252167815721513,
10.0953744497603));
#11048=CARTESIAN_POINT('Ctrl Pts',(-0.737873175341583,-0.689832624733134,
10.1188030808968));
#11049=CARTESIAN_POINT('Ctrl Pts',(-0.318698452927423,-0.960430879264268,
10.1422781619728));
#11050=CARTESIAN_POINT('Ctrl Pts',(0.179821322079405,-0.997802115099903,
10.165801016687));
#11051=CARTESIAN_POINT('Ctrl Pts',(0.569799688583804,-0.821825224718302,
10.1859332990401));
#11052=CARTESIAN_POINT('Ctrl Pts',(0.808529272399683,-0.568786525126624,
10.2026554795479));
#11053=CARTESIAN_POINT('Ctrl Pts',(0.978302334856632,-0.241355508961501,
10.2203816226583));
#11054=CARTESIAN_POINT('Ctrl Pts',(1.00538906456187,0.2333495834722,10.2425768960728));
#11055=CARTESIAN_POINT('Ctrl Pts',(0.728694779250168,0.734236927042486,
10.2692732222169));
#11056=CARTESIAN_POINT('Ctrl Pts',(0.226966011237296,1.01173169163385,10.2960314782446));
#11057=CARTESIAN_POINT('Ctrl Pts',(-0.346931921015741,0.979703466525211,
10.322852197852));
#11058=CARTESIAN_POINT('Ctrl Pts',(-0.816881713892654,0.64646497162191,
10.3497355932434));
#11059=CARTESIAN_POINT('Ctrl Pts',(-1.03804453245733,0.113033933490282,
10.3766819555363));
#11060=CARTESIAN_POINT('Ctrl Pts',(-0.941273337654569,-0.457636831985297,
10.4036914771008));
#11061=CARTESIAN_POINT('Ctrl Pts',(-0.554821661701358,-0.890363150138494,
10.4307643281566));
#11062=CARTESIAN_POINT('Ctrl Pts',(0.0039266343485537,-1.05153545558377,
10.4579006219194));
#11063=CARTESIAN_POINT('Ctrl Pts',(0.56408641499002,-0.890355693773659,
10.4851004304633));
#11064=CARTESIAN_POINT('Ctrl Pts',(0.95354049595536,-0.454843948120234,
10.5123637773334));
#11065=CARTESIAN_POINT('Ctrl Pts',(1.05182093126769,0.122456968256553,10.5396906391692));
#11066=CARTESIAN_POINT('Ctrl Pts',(0.827373278245085,0.664814101527569,
10.5670809495482));
#11067=CARTESIAN_POINT('Ctrl Pts',(0.347668418055166,1.00541156633213,10.5945345871301));
#11068=CARTESIAN_POINT('Ctrl Pts',(-0.241071265795766,1.03865810273544,
10.622051404586));
#11069=CARTESIAN_POINT('Ctrl Pts',(-0.758443515163291,0.752928057938471,
10.6496311647854));
#11070=CARTESIAN_POINT('Ctrl Pts',(-1.04515215340155,0.234550923711717,
10.6772736879972));
#11071=CARTESIAN_POINT('Ctrl Pts',(-1.01205642652925,-0.35823601679832,
10.704978520474));
#11072=CARTESIAN_POINT('Ctrl Pts',(-0.66789446460778,-0.843672061466428,
10.7327456863726));
#11073=CARTESIAN_POINT('Ctrl Pts',(-0.11702199962579,-1.07205102198006,
10.7605740118105));
#11074=CARTESIAN_POINT('Ctrl Pts',(0.472188983917981,-0.972273573004842,
10.7884648797228));
#11075=CARTESIAN_POINT('Ctrl Pts',(0.91890408267479,-0.573161580699387,
10.8164138322953));
#11076=CARTESIAN_POINT('Ctrl Pts',(1.02972492095809,-0.189114130706034,
10.8350920076366));
#11077=CARTESIAN_POINT('Ctrl Pts',(1.02975090409547,0.00389522410502781,
10.8444331682177));
#11078=CARTESIAN_POINT('Ctrl Pts',(1.03719645688851,-0.0037293349184744,
7.95215989910766));
#11079=CARTESIAN_POINT('Ctrl Pts',(1.03717028584552,0.190675813657207,7.96156861253759));
#11080=CARTESIAN_POINT('Ctrl Pts',(0.925557950139338,0.577535603721514,
7.98038266347121));
#11081=CARTESIAN_POINT('Ctrl Pts',(0.475545581675125,0.979605390126322,
8.00853780142747));
#11082=CARTESIAN_POINT('Ctrl Pts',(-0.118073456635005,1.08013597304276,
8.03663686932194));
#11083=CARTESIAN_POINT('Ctrl Pts',(-0.67312151375956,0.850028585888234,
8.06467548649113));
#11084=CARTESIAN_POINT('Ctrl Pts',(-1.01992165763532,0.360873298516457,
8.09265479891218));
#11085=CARTESIAN_POINT('Ctrl Pts',(-1.05327498416264,-0.236503717327239,
8.12057352562096));
#11086=CARTESIAN_POINT('Ctrl Pts',(-0.764326765396757,-0.758933398467517,
8.14843151942941));
#11087=CARTESIAN_POINT('Ctrl Pts',(-0.24287688627644,-1.04691794387519,
8.17622817905231));
#11088=CARTESIAN_POINT('Ctrl Pts',(0.350539555856497,-1.01340964671441,
8.20396316269724));
#11089=CARTESIAN_POINT('Ctrl Pts',(0.834083805209005,-0.670091304275385,
8.23163607534286));
#11090=CARTESIAN_POINT('Ctrl Pts',(1.06033935713661,-0.123370274675711,
8.25924660824643));
#11091=CARTESIAN_POINT('Ctrl Pts',(0.961271344301675,0.458596094063279,
8.28679447706705));
#11092=CARTESIAN_POINT('Ctrl Pts',(0.568649593858113,0.89765324776651,8.31427945443487));
#11093=CARTESIAN_POINT('Ctrl Pts',(0.0039431239572611,1.06012773827784,
8.34170134991208));
#11094=CARTESIAN_POINT('Ctrl Pts',(-0.559405334450464,0.897668914802851,
8.36906003124174));
#11095=CARTESIAN_POINT('Ctrl Pts',(-0.9344966664178,0.477459366698196,8.39534445047533));
#11096=CARTESIAN_POINT('Ctrl Pts',(-1.02319118570897,0.0361130383904124,
8.41652764356969));
#11097=CARTESIAN_POINT('Ctrl Pts',(-0.972095066647408,-0.252162816722124,
8.43062781257449));
#11098=CARTESIAN_POINT('Ctrl Pts',(-0.913310980160994,-0.40757250314265,
8.43867876960068));
#11099=CARTESIAN_POINT('Ctrl Pts',(-0.796998155287066,-0.627946628775765,
8.45074896302428));
#11100=CARTESIAN_POINT('Ctrl Pts',(-0.5220491698584,-0.896088884437607,
8.46883099651776));
#11101=CARTESIAN_POINT('Ctrl Pts',(-0.0296099107857316,-1.03488745726812,
8.49289019054928));
#11102=CARTESIAN_POINT('Ctrl Pts',(0.467306135314492,-0.920636354183639,
8.516899481238));
#11103=CARTESIAN_POINT('Ctrl Pts',(0.913883301313135,-0.528332204193271,
8.54485233012596));
#11104=CARTESIAN_POINT('Ctrl Pts',(1.07128001712609,0.1578675794943,8.57671607247633));
#11105=CARTESIAN_POINT('Ctrl Pts',(0.718979530768331,0.764750753676088,
8.60848123379351));
#11106=CARTESIAN_POINT('Ctrl Pts',(0.181072046006281,1.00590047741433,8.63620356340674));
#11107=CARTESIAN_POINT('Ctrl Pts',(-0.321113972152043,0.968286917313835,
8.65991664175283));
#11108=CARTESIAN_POINT('Ctrl Pts',(-0.708570956654293,0.717751349650519,
8.68160963014022));
#11109=CARTESIAN_POINT('Ctrl Pts',(-0.927415223878402,0.368253958999767,
8.70129511507728));
#11110=CARTESIAN_POINT('Ctrl Pts',(-1.02080929264471,-0.117772384129308,
8.72488167062357));
#11111=CARTESIAN_POINT('Ctrl Pts',(-0.784094990025882,-0.722349424629435,
8.75429895428144));
#11112=CARTESIAN_POINT('Ctrl Pts',(-0.0826159953470804,-1.05973861779947,
8.78949320300836));
#11113=CARTESIAN_POINT('Ctrl Pts',(0.657991980809365,-0.830533515786699,
8.82458319261689));
#11114=CARTESIAN_POINT('Ctrl Pts',(1.04435983522905,-0.161028240208566,
8.85957047777063));
#11115=CARTESIAN_POINT('Ctrl Pts',(0.872191510918413,0.591096145520318,
8.89445647423708));
#11116=CARTESIAN_POINT('Ctrl Pts',(0.342833637985558,0.950500175170697,
8.92344635583295));
#11117=CARTESIAN_POINT('Ctrl Pts',(-0.14240681866231,0.967149549215652,
8.94658832164588));
#11118=CARTESIAN_POINT('Ctrl Pts',(-0.523468734534486,0.83435343134501,
8.96584682092899));
#11119=CARTESIAN_POINT('Ctrl Pts',(-0.845308154191094,0.520393139588824,
8.98699752602333));
#11120=CARTESIAN_POINT('Ctrl Pts',(-0.989543012390118,0.0525630321306637,
9.01003011003576));
#11121=CARTESIAN_POINT('Ctrl Pts',(-0.892450536231069,-0.426209645755978,
9.03302022621514));
#11122=CARTESIAN_POINT('Ctrl Pts',(-0.578881824747128,-0.799912768402463,
9.05597195626933));
#11123=CARTESIAN_POINT('Ctrl Pts',(-0.125687474439124,-0.977501797786432,
9.07888255350409));
#11124=CARTESIAN_POINT('Ctrl Pts',(0.316605904211817,-0.92198833082841,
9.09984979011061));
#11125=CARTESIAN_POINT('Ctrl Pts',(0.653671319469926,-0.709225736145728,
9.11888250352145));
#11126=CARTESIAN_POINT('Ctrl Pts',(0.939439239276747,-0.325183836095085,
9.14169385358281));
#11127=CARTESIAN_POINT('Ctrl Pts',(0.987547025680681,0.301278408095195,
9.17015565689872));
#11128=CARTESIAN_POINT('Ctrl Pts',(0.594679321542008,0.791379583113645,
9.19855495717846));
#11129=CARTESIAN_POINT('Ctrl Pts',(0.145457247238317,0.946900230408442,
9.22123290378143));
#11130=CARTESIAN_POINT('Ctrl Pts',(-0.269744512554461,0.932152140919955,
9.24105448849287));
#11131=CARTESIAN_POINT('Ctrl Pts',(-0.694101106221571,0.697615963332633,
9.26367797146862));
#11132=CARTESIAN_POINT('Ctrl Pts',(-0.957289766597392,0.221074138858957,
9.28908905057342));
#11133=CARTESIAN_POINT('Ctrl Pts',(-0.926805285883287,-0.322025406634136,
9.3144611162));
#11134=CARTESIAN_POINT('Ctrl Pts',(-0.670552563620864,-0.682150076663051,
9.33510504039983));
#11135=CARTESIAN_POINT('Ctrl Pts',(-0.321671655798842,-0.895341345847391,
9.35478847828045));
#11136=CARTESIAN_POINT('Ctrl Pts',(0.0307752103413157,-0.957613220501112,
9.37164419348245));
#11137=CARTESIAN_POINT('Ctrl Pts',(0.409786204776528,-0.855569172091428,
9.39035412038357));
#11138=CARTESIAN_POINT('Ctrl Pts',(0.693500977439743,-0.646372437096977,
9.40717726375736));
#11139=CARTESIAN_POINT('Ctrl Pts',(0.880977325954236,-0.347876678883315,
9.42398736672525));
#11140=CARTESIAN_POINT('Ctrl Pts',(0.940946228891237,-0.0307571479885627,
9.43938348179057));
#11141=CARTESIAN_POINT('Ctrl Pts',(0.900090933330989,0.257284228276144,
9.45336988898821));
#11142=CARTESIAN_POINT('Ctrl Pts',(0.75789942871261,0.576053653419727,9.47014345990121));
#11143=CARTESIAN_POINT('Ctrl Pts',(0.423486133635302,0.87520526392437,9.49109488900207));
#11144=CARTESIAN_POINT('Ctrl Pts',(-0.107317293259283,0.965309921368965,
9.51620779009144));
#11145=CARTESIAN_POINT('Ctrl Pts',(-0.520902213846082,0.793666918986136,
9.53711515836644));
#11146=CARTESIAN_POINT('Ctrl Pts',(-0.759397793029819,0.54064129614791,
9.55382724163822));
#11147=CARTESIAN_POINT('Ctrl Pts',(-0.919357990870187,0.232108695129427,
9.57053164436102));
#11148=CARTESIAN_POINT('Ctrl Pts',(-0.944612254049654,-0.214222806773856,
9.59140013603058));
#11149=CARTESIAN_POINT('Ctrl Pts',(-0.685107321886509,-0.683500930880567,
9.61642055252469));
#11150=CARTESIAN_POINT('Ctrl Pts',(-0.216252770756576,-0.942567517453279,
9.6414222205253));
#11151=CARTESIAN_POINT('Ctrl Pts',(0.318278561645482,-0.912511970668242,
9.66640623507196));
#11152=CARTESIAN_POINT('Ctrl Pts',(0.754581459699137,-0.602868595837562,
9.69137453525599));
#11153=CARTESIAN_POINT('Ctrl Pts',(0.959169418745129,-0.108840250447074,
9.7163286998096));
#11154=CARTESIAN_POINT('Ctrl Pts',(0.869615683384371,0.418055869863705,
9.74127046801076));
#11155=CARTESIAN_POINT('Ctrl Pts',(0.513593683823807,0.816378372045758,
9.7662015614447));
#11156=CARTESIAN_POINT('Ctrl Pts',(0.000472864523384456,0.964194355862096,
9.7911236329607));
#11157=CARTESIAN_POINT('Ctrl Pts',(-0.512639156114366,0.816398384562372,
9.8160385797356));
#11158=CARTESIAN_POINT('Ctrl Pts',(-0.854897593072207,0.433135404547336,
9.84002524516739));
#11159=CARTESIAN_POINT('Ctrl Pts',(-0.951920813198652,-0.0473618249043272,
9.86308637136708));
#11160=CARTESIAN_POINT('Ctrl Pts',(-0.813150828637682,-0.496663759626729,
9.8852216709568));
#11161=CARTESIAN_POINT('Ctrl Pts',(-0.504527693025104,-0.797911067211824,
9.90551184440933));
#11162=CARTESIAN_POINT('Ctrl Pts',(-0.139592336256419,-0.924897874793092,
9.9239588016233));
#11163=CARTESIAN_POINT('Ctrl Pts',(0.32476002062656,-0.908862355890077,
9.94609483836991));
#11164=CARTESIAN_POINT('Ctrl Pts',(0.728526143184254,-0.634941072206952,
9.96823570550932));
#11165=CARTESIAN_POINT('Ctrl Pts',(0.912651243172658,-0.207993974856502,
9.9903798965011));
#11166=CARTESIAN_POINT('Ctrl Pts',(0.93159093211479,0.255865599740591,10.0125272672192));
#11167=CARTESIAN_POINT('Ctrl Pts',(0.626775516099417,0.785983302959022,
10.0402233323282));
#11168=CARTESIAN_POINT('Ctrl Pts',(-0.0764260103068494,1.00290823265387,
10.0734741130373));
#11169=CARTESIAN_POINT('Ctrl Pts',(-0.663913049810778,0.718917831796266,
10.1030507684028));
#11170=CARTESIAN_POINT('Ctrl Pts',(-0.926512975578048,0.234583456765021,
10.1289456687419));
#11171=CARTESIAN_POINT('Ctrl Pts',(-0.926479271132153,-0.236978839253667,
10.1511526887213));
#11172=CARTESIAN_POINT('Ctrl Pts',(-0.700839853017446,-0.652019794966121,
10.1733738737333));
#11173=CARTESIAN_POINT('Ctrl Pts',(-0.303776802726922,-0.908251612454935,
10.1956106345133));
#11174=CARTESIAN_POINT('Ctrl Pts',(0.167783237861881,-0.943528965310917,
10.2178619614777));
#11175=CARTESIAN_POINT('Ctrl Pts',(0.536202295862543,-0.777216710409037,
10.2368850275763));
#11176=CARTESIAN_POINT('Ctrl Pts',(0.76151294157343,-0.538381201717669,
10.2526688564185));
#11177=CARTESIAN_POINT('Ctrl Pts',(0.921632025245598,-0.229535734594294,
10.2693891391398));
#11178=CARTESIAN_POINT('Ctrl Pts',(0.947080496251134,0.217794926170324,
10.2903068420048));
#11179=CARTESIAN_POINT('Ctrl Pts',(0.686598901099996,0.689141902373008,
10.3154333425304));
#11180=CARTESIAN_POINT('Ctrl Pts',(0.214945265052869,0.94990696216286,10.3405880336628));
#11181=CARTESIAN_POINT('Ctrl Pts',(-0.323876018866969,0.919752968003473,
10.3657719058747));
#11182=CARTESIAN_POINT('Ctrl Pts',(-0.764572616499986,0.607160410323047,
10.3909867552046));
#11183=CARTESIAN_POINT('Ctrl Pts',(-0.971702406404501,0.107377544455468,
10.4162339680835));
#11184=CARTESIAN_POINT('Ctrl Pts',(-0.881059610722316,-0.426720480341076,
10.4415150769132));
#11185=CARTESIAN_POINT('Ctrl Pts',(-0.519655694997322,-0.831297350140601,
10.4668315108411));
#11186=CARTESIAN_POINT('Ctrl Pts',(0.00235883360422653,-0.98180710952777,
10.4921846931895));
#11187=CARTESIAN_POINT('Ctrl Pts',(0.525223150865608,-0.831296672923994,
10.5175760215671));
#11188=CARTESIAN_POINT('Ctrl Pts',(0.888435991055881,-0.425046664919749,
10.5430068558293));
#11189=CARTESIAN_POINT('Ctrl Pts',(0.979988661732392,0.113038466202106,
10.5684785338995));
#11190=CARTESIAN_POINT('Ctrl Pts',(0.770886513678643,0.618192706747942,
10.5939923551312));
#11191=CARTESIAN_POINT('Ctrl Pts',(0.324317244435882,0.935211426154897,
10.6195495969629));
#11192=CARTESIAN_POINT('Ctrl Pts',(-0.22342646197345,0.966104184880575,
10.6451514997004));
#11193=CARTESIAN_POINT('Ctrl Pts',(-0.704517100257862,0.700372287633452,
10.6707992716954));
#11194=CARTESIAN_POINT('Ctrl Pts',(-0.970986492881063,0.218523865304527,
10.6964940855284));
#11195=CARTESIAN_POINT('Ctrl Pts',(-0.940209380211664,-0.332262593742652,
10.7222371038369));
#11196=CARTESIAN_POINT('Ctrl Pts',(-0.620514508604514,-0.783155463378012,
10.7480293919687));
#11197=CARTESIAN_POINT('Ctrl Pts',(-0.10896221887375,-0.995208970605426,
10.7738721348519));
#11198=CARTESIAN_POINT('Ctrl Pts',(0.43807428354937,-0.902589090530947,
10.7997661462395));
#11199=CARTESIAN_POINT('Ctrl Pts',(0.85274473405393,-0.532059372519866,
10.8257129556942));
#11200=CARTESIAN_POINT('Ctrl Pts',(0.955606232646419,-0.175711702508772,
10.8430448118064));
#11201=CARTESIAN_POINT('Ctrl Pts',(0.955630365396176,0.00355250229995129,
10.8517207421788));
#11202=CARTESIAN_POINT('Ctrl Pts',(1.0838482003043,-0.000914448548792532,
7.89412779065783));
#11203=CARTESIAN_POINT('Ctrl Pts',(1.08382086259523,0.202156991753356,7.90395593050703));
#11204=CARTESIAN_POINT('Ctrl Pts',(0.96716342125297,0.606732997046235,7.92363301940144));
#11205=CARTESIAN_POINT('Ctrl Pts',(0.496000875527845,1.02784680220822,7.95311729373211));
#11206=CARTESIAN_POINT('Ctrl Pts',(-0.126541219357233,1.13341877234435,
7.98258888834162));
#11207=CARTESIAN_POINT('Ctrl Pts',(-0.709545608469748,0.891862572219048,
8.01203898822628));
#11208=CARTESIAN_POINT('Ctrl Pts',(-1.07441005641409,0.377463005767994,
8.04146921435643));
#11209=CARTESIAN_POINT('Ctrl Pts',(-1.10966865400436,-0.251710046816853,
8.07087652363246));
#11210=CARTESIAN_POINT('Ctrl Pts',(-0.805032466753758,-0.80276307880036,
8.10025997100121));
#11211=CARTESIAN_POINT('Ctrl Pts',(-0.254398208228186,-1.10700349947945,
8.12961768909314));
#11212=CARTESIAN_POINT('Ctrl Pts',(0.373117719641826,-1.07168631577933,
8.15894823924168));
#11213=CARTESIAN_POINT('Ctrl Pts',(0.88515438734053,-0.708276627835562,
8.18825002300904));
#11214=CARTESIAN_POINT('Ctrl Pts',(1.12510635980224,-0.128745368292323,
8.21752154423205));
#11215=CARTESIAN_POINT('Ctrl Pts',(1.02006457029756,0.488942832092543,8.24676128145543));
#11216=CARTESIAN_POINT('Ctrl Pts',(0.602951017257973,0.95554132784791,8.27596778161598));
#11217=CARTESIAN_POINT('Ctrl Pts',(0.00226783791176727,1.12846883942168,
8.30513956604923));
#11218=CARTESIAN_POINT('Ctrl Pts',(-0.597667353003912,0.955557647790115,
8.33427528667529));
#11219=CARTESIAN_POINT('Ctrl Pts',(-0.997580811393811,0.507673638651765,
8.36229572045689));
#11220=CARTESIAN_POINT('Ctrl Pts',(-1.09227219135141,0.0367679381382032,
8.38489914841893));
#11221=CARTESIAN_POINT('Ctrl Pts',(-1.03772824844162,-0.271014548929116,
8.39995360230054));
#11222=CARTESIAN_POINT('Ctrl Pts',(-0.974949204552547,-0.436989591216038,
8.40855194537982));
#11223=CARTESIAN_POINT('Ctrl Pts',(-0.850705795757624,-0.672393715416174,
8.42144546139659));
#11224=CARTESIAN_POINT('Ctrl Pts',(-0.556878890231008,-0.959006027648614,
8.44077179267571));
#11225=CARTESIAN_POINT('Ctrl Pts',(-0.0301913926151124,-1.10751276767793,
8.46650528584973));
#11226=CARTESIAN_POINT('Ctrl Pts',(0.501708333376544,-0.98527102028979,
8.49220475204497));
#11227=CARTESIAN_POINT('Ctrl Pts',(0.980083971872979,-0.565112204961699,
8.52214616157649));
#11228=CARTESIAN_POINT('Ctrl Pts',(1.14895607407238,0.170475723569411,8.55630580617952));
#11229=CARTESIAN_POINT('Ctrl Pts',(0.7710459574588,0.821732127342494,8.59039054363123));
#11230=CARTESIAN_POINT('Ctrl Pts',(0.193487242513833,1.08070806313451,8.62015730147285));
#11231=CARTESIAN_POINT('Ctrl Pts',(-0.346009171336449,1.04033345516453,
8.64563214466693));
#11232=CARTESIAN_POINT('Ctrl Pts',(-0.762466515394437,0.771083934602891,
8.66894777270452));
#11233=CARTESIAN_POINT('Ctrl Pts',(-0.99778215525873,0.395306289766034,
8.69011375490029));
#11234=CARTESIAN_POINT('Ctrl Pts',(-1.0982483309166,-0.127426784513864,
8.71548185859923));
#11235=CARTESIAN_POINT('Ctrl Pts',(-0.843613153081136,-0.777967142474131,
8.74713381288415));
#11236=CARTESIAN_POINT('Ctrl Pts',(-0.088507342272469,-1.14122962611758,
8.78501928785707));
#11237=CARTESIAN_POINT('Ctrl Pts',(0.709065757260984,-0.894452196565483,
8.82280637288963));
#11238=CARTESIAN_POINT('Ctrl Pts',(1.12529561032464,-0.173286632271806,
8.86049290545786));
#11239=CARTESIAN_POINT('Ctrl Pts',(0.939827863300308,0.637049421449346,
8.89807721520378));
#11240=CARTESIAN_POINT('Ctrl Pts',(0.369468399528226,1.02430481692951,8.92931078741886));
#11241=CARTESIAN_POINT('Ctrl Pts',(-0.15336583993037,1.0422444816976,8.95424500292052));
#11242=CARTESIAN_POINT('Ctrl Pts',(-0.563936805331798,0.899166803592543,
8.97499399053462));
#11243=CARTESIAN_POINT('Ctrl Pts',(-0.910669570745192,0.560918417615995,
8.99777978341788));
#11244=CARTESIAN_POINT('Ctrl Pts',(-1.06604101086678,0.0569636584812059,
9.02258893664379));
#11245=CARTESIAN_POINT('Ctrl Pts',(-0.961451537401035,-0.458702011613492,
9.0473503347936));
#11246=CARTESIAN_POINT('Ctrl Pts',(-0.623794994012935,-0.861102456908409,
9.0720625968117));
#11247=CARTESIAN_POINT('Ctrl Pts',(-0.135894920546228,-1.05227024528694,
9.0967266248224));
#11248=CARTESIAN_POINT('Ctrl Pts',(0.340102284602575,-0.992509712058549,
9.11928978647568));
#11249=CARTESIAN_POINT('Ctrl Pts',(0.702746144635939,-0.763590236431144,
9.13976608516106));
#11250=CARTESIAN_POINT('Ctrl Pts',(1.01011084241462,-0.350500037079963,
9.16430047463988));
#11251=CARTESIAN_POINT('Ctrl Pts',(1.0617514972005,0.323027753091657,9.19489901500147));
#11252=CARTESIAN_POINT('Ctrl Pts',(0.639624221556973,0.84946830932992,9.22540199762321));
#11253=CARTESIAN_POINT('Ctrl Pts',(0.157300877416754,1.01642810811852,9.24974966923183));
#11254=CARTESIAN_POINT('Ctrl Pts',(-0.288301982182871,1.00058338021818,
9.27102081642107));
#11255=CARTESIAN_POINT('Ctrl Pts',(-0.743430664340233,0.74898609481149,
9.29528306623843));
#11256=CARTESIAN_POINT('Ctrl Pts',(-1.02546174642978,0.238215657258133,
9.32251462671953));
#11257=CARTESIAN_POINT('Ctrl Pts',(-0.992748476251999,-0.343390555439158,
9.34968277653113));
#11258=CARTESIAN_POINT('Ctrl Pts',(-0.718527463530067,-0.728675713878542,
9.37176741485846));
#11259=CARTESIAN_POINT('Ctrl Pts',(-0.345458809407523,-0.956634300940651,
9.39281388741142));
#11260=CARTESIAN_POINT('Ctrl Pts',(0.0311884895998242,-1.02314357299083,
9.41082562368356));
#11261=CARTESIAN_POINT('Ctrl Pts',(0.435880506281094,-0.914158731694693,
9.43080150015021));
#11262=CARTESIAN_POINT('Ctrl Pts',(0.738620974493306,-0.690909070523313,
9.44875254494689));
#11263=CARTESIAN_POINT('Ctrl Pts',(0.9385024099283,-0.372611741600812,9.46667467159655));
#11264=CARTESIAN_POINT('Ctrl Pts',(1.00237872112136,-0.0347073992703695,
9.48307805826784));
#11265=CARTESIAN_POINT('Ctrl Pts',(0.958861569486603,0.272010577946869,
9.49797018640025));
#11266=CARTESIAN_POINT('Ctrl Pts',(0.807519793645455,0.611255165848026,
9.51582019885214));
#11267=CARTESIAN_POINT('Ctrl Pts',(0.451909976937506,0.929265184877128,
9.53809184874244));
#11268=CARTESIAN_POINT('Ctrl Pts',(-0.111797110794033,1.0248480893635,9.56475740718536));
#11269=CARTESIAN_POINT('Ctrl Pts',(-0.550390920642296,0.842725120389943,
9.58692643984169));
#11270=CARTESIAN_POINT('Ctrl Pts',(-0.803077343857937,0.574617344448347,
9.60463278999863));
#11271=CARTESIAN_POINT('Ctrl Pts',(-0.97243696867917,0.247916429508408,
9.62231887693885));
#11272=CARTESIAN_POINT('Ctrl Pts',(-0.999058693555682,-0.224167470527981,
9.64438690207702));
#11273=CARTESIAN_POINT('Ctrl Pts',(-0.724871986515919,-0.719760375599744,
9.6708095787426));
#11274=CARTESIAN_POINT('Ctrl Pts',(-0.230348354153974,-0.992872189570322,
9.69717262938872));
#11275=CARTESIAN_POINT('Ctrl Pts',(0.332515958586368,-0.961100479168014,
9.72347720468563));
#11276=CARTESIAN_POINT('Ctrl Pts',(0.791156172152085,-0.635448799884614,
9.74972373646253));
#11277=CARTESIAN_POINT('Ctrl Pts',(1.00578640215473,-0.116833985348966,
9.77591303739745));
#11278=CARTESIAN_POINT('Ctrl Pts',(0.911811450066463,0.435293222025004,
9.80204583327431));
#11279=CARTESIAN_POINT('Ctrl Pts',(0.539261434877731,0.851908601823872,
9.82812290732319));
#11280=CARTESIAN_POINT('Ctrl Pts',(0.00336028235764251,1.00614792986501,
9.85414516087386));
#11281=CARTESIAN_POINT('Ctrl Pts',(-0.531503227958469,0.851946292011022,
9.88011328551953));
#11282=CARTESIAN_POINT('Ctrl Pts',(-0.887541808641719,0.453048239768111,
9.90506874294698));
#11283=CARTESIAN_POINT('Ctrl Pts',(-0.988224862711454,-0.0460782804447304,
9.92901840717504));
#11284=CARTESIAN_POINT('Ctrl Pts',(-0.844211613760868,-0.511992487885777,
9.95197147120267));
#11285=CARTESIAN_POINT('Ctrl Pts',(-0.52463839039403,-0.823802817820016,
9.9729753411795));
#11286=CARTESIAN_POINT('Ctrl Pts',(-0.147402040593785,-0.955022699264225,
9.99204031078243));
#11287=CARTESIAN_POINT('Ctrl Pts',(0.331994552727527,-0.938394674293537,
10.0148912553923));
#11288=CARTESIAN_POINT('Ctrl Pts',(0.747859600288323,-0.655983436748773,
10.0376971514725));
#11289=CARTESIAN_POINT('Ctrl Pts',(0.937105692798899,-0.216960017735763,
10.0604636979959));
#11290=CARTESIAN_POINT('Ctrl Pts',(0.956494142862348,0.259388583755504,
10.0832041717988));
#11291=CARTESIAN_POINT('Ctrl Pts',(0.643862373212363,0.802456461011887,
10.1115758852511));
#11292=CARTESIAN_POINT('Ctrl Pts',(-0.0748631700336077,1.02374906025246,
10.1455482688799));
#11293=CARTESIAN_POINT('Ctrl Pts',(-0.673362689405438,0.734057071294702,
10.1756792735207));
#11294=CARTESIAN_POINT('Ctrl Pts',(-0.940211173985656,0.241612490483782,
10.2020001217299));
#11295=CARTESIAN_POINT('Ctrl Pts',(-0.940061131273621,-0.236900273902396,
10.2245322988002));
#11296=CARTESIAN_POINT('Ctrl Pts',(-0.711446123935283,-0.657195553614125,
10.247034622298));
#11297=CARTESIAN_POINT('Ctrl Pts',(-0.310032668855504,-0.916099462990559,
10.2695077971124));
#11298=CARTESIAN_POINT('Ctrl Pts',(0.165734041548867,-0.951573099062055,
10.291955877611));
#11299=CARTESIAN_POINT('Ctrl Pts',(0.536637465797884,-0.78402716349881,
10.311104963167));
#11300=CARTESIAN_POINT('Ctrl Pts',(0.76314851915361,-0.543880336389376,
10.3269730190361));
#11301=CARTESIAN_POINT('Ctrl Pts',(0.923937995332574,-0.233678441944692,
10.3437641472873));
#11302=CARTESIAN_POINT('Ctrl Pts',(0.949313105102571,0.214827832547124,
10.3647313433219));
#11303=CARTESIAN_POINT('Ctrl Pts',(0.688565919279137,0.686304166961507,
10.389864829251));
#11304=CARTESIAN_POINT('Ctrl Pts',(0.217650841892384,0.946463195692629,
10.4149706945773));
#11305=CARTESIAN_POINT('Ctrl Pts',(-0.319048217451104,0.916258727218333,
10.440051304975));
#11306=CARTESIAN_POINT('Ctrl Pts',(-0.756961259842281,0.605434323983068,
10.4651078480003));
#11307=CARTESIAN_POINT('Ctrl Pts',(-0.962226484778156,0.109716966678491,
10.4901420759625));
#11308=CARTESIAN_POINT('Ctrl Pts',(-0.872365348998548,-0.418790659164996,
10.5151555282894));
#11309=CARTESIAN_POINT('Ctrl Pts',(-0.515377026932851,-0.818178757886243,
10.5401498745057));
#11310=CARTESIAN_POINT('Ctrl Pts',(-0.000980240333085043,-0.966322769852347,
10.5651267379984));
#11311=CARTESIAN_POINT('Ctrl Pts',(0.513063068024907,-0.818183101349432,
10.5900878010138));
#11312=CARTESIAN_POINT('Ctrl Pts',(0.869301976324407,-0.419491985735566,
10.6150347288481));
#11313=CARTESIAN_POINT('Ctrl Pts',(0.958780479694553,0.1073556061531,10.6399692179751));
#11314=CARTESIAN_POINT('Ctrl Pts',(0.754335676381123,0.600843600178277,
10.6648929541654));
#11315=CARTESIAN_POINT('Ctrl Pts',(0.318834621372516,0.90981229213662,10.6898076577536));
#11316=CARTESIAN_POINT('Ctrl Pts',(-0.214141831829799,0.939716543474692,
10.7147150160685));
#11317=CARTESIAN_POINT('Ctrl Pts',(-0.681238257715304,0.68154065932501,
10.7396167908086));
#11318=CARTESIAN_POINT('Ctrl Pts',(-0.939353232681883,0.214492092469083,
10.7645145830463));
#11319=CARTESIAN_POINT('Ctrl Pts',(-0.909441174443961,-0.318236929963865,
10.7894103781415));
#11320=CARTESIAN_POINT('Ctrl Pts',(-0.600708513133185,-0.753434977070502,
10.8143052762627));
#11321=CARTESIAN_POINT('Ctrl Pts',(-0.107767289636025,-0.957617587334566,
10.8392023443988));
#11322=CARTESIAN_POINT('Ctrl Pts',(0.418292015354745,-0.868431439290108,
10.8641002181391));
#11323=CARTESIAN_POINT('Ctrl Pts',(0.816252889411692,-0.512592296203714,
10.8890073890965));
#11324=CARTESIAN_POINT('Ctrl Pts',(0.914688282568999,-0.171209962575356,
10.9056065352154));
#11325=CARTESIAN_POINT('Ctrl Pts',(0.914711404788378,0.000547765501091019,
10.9139191712561));
#11326=CARTESIAN_POINT('Ctrl Pts',(1.06701743632438,0.0025960290114382,
7.82154662476291));
#11327=CARTESIAN_POINT('Ctrl Pts',(1.06699050603538,0.202641049598823,7.83122829361572));
#11328=CARTESIAN_POINT('Ctrl Pts',(0.952169403602462,0.601316966034855,
7.850613547215));
#11329=CARTESIAN_POINT('Ctrl Pts',(0.487093861785577,1.01725013287211,7.87972343428257));
#11330=CARTESIAN_POINT('Ctrl Pts',(-0.128666178509213,1.12181753997798,
7.90887159798562));
#11331=CARTESIAN_POINT('Ctrl Pts',(-0.706490994785343,0.882579858430546,
7.93805444725339));
#11332=CARTESIAN_POINT('Ctrl Pts',(-1.06888045229236,0.371930676583893,
7.96727152805071));
#11333=CARTESIAN_POINT('Ctrl Pts',(-1.10411045676727,-0.253923420995056,
7.99652093475803));
#11334=CARTESIAN_POINT('Ctrl Pts',(-0.800647763134568,-0.803185289622725,
8.02580137401769));
#11335=CARTESIAN_POINT('Ctrl Pts',(-0.250930641224358,-1.10710470404373,
8.05511124460616));
#11336=CARTESIAN_POINT('Ctrl Pts',(0.376814540590657,-1.07193905643761,
8.08444904323414));
#11337=CARTESIAN_POINT('Ctrl Pts',(0.890086824381486,-0.707854158546105,
8.11381319934604));
#11338=CARTESIAN_POINT('Ctrl Pts',(1.13117627450501,-0.126006039541308,
8.14320213996355));
#11339=CARTESIAN_POINT('Ctrl Pts',(1.02566796039198,0.495407813750173,8.17261426104031));
#11340=CARTESIAN_POINT('Ctrl Pts',(0.605395747600651,0.965787356705992,
8.20204794473113));
#11341=CARTESIAN_POINT('Ctrl Pts',(-0.00109610972165227,1.14055805748304,
8.2315015642435));
#11342=CARTESIAN_POINT('Ctrl Pts',(-0.608048139592871,0.965796133351913,
8.26097343779502));
#11343=CARTESIAN_POINT('Ctrl Pts',(-1.01347415035759,0.51197072632285,8.28936978311824));
#11344=CARTESIAN_POINT('Ctrl Pts',(-1.10970380118711,0.033896466150247,
8.31231621328207));
#11345=CARTESIAN_POINT('Ctrl Pts',(-1.05427292616554,-0.27897678633527,
8.32761884188052));
#11346=CARTESIAN_POINT('Ctrl Pts',(-0.990418366398432,-0.447799765271943,
8.33636455425477));
#11347=CARTESIAN_POINT('Ctrl Pts',(-0.863997036800892,-0.68734004421506,
8.34948431630875));
#11348=CARTESIAN_POINT('Ctrl Pts',(-0.56477516495449,-0.97932462816657,
8.3691676579603));
#11349=CARTESIAN_POINT('Ctrl Pts',(-0.0274664722784836,-1.13095114472672,
8.39542113766043));
#11350=CARTESIAN_POINT('Ctrl Pts',(0.516092848385612,-1.00613117413851,
8.42168142940329));
#11351=CARTESIAN_POINT('Ctrl Pts',(1.0057877897569,-0.576213269843886,8.45232537141141));
#11352=CARTESIAN_POINT('Ctrl Pts',(1.17928912153765,0.178065478023402,8.48735422482944));
#11353=CARTESIAN_POINT('Ctrl Pts',(0.791104418082697,0.847685062285886,
8.52238889521533));
#11354=CARTESIAN_POINT('Ctrl Pts',(0.196290711324304,1.11453858289063,8.5530461496888));
#11355=CARTESIAN_POINT('Ctrl Pts',(-0.360219354067838,1.0729904639039,8.5793236664903));
#11356=CARTESIAN_POINT('Ctrl Pts',(-0.790510042128262,0.794916107930365,
8.60341001062862));
#11357=CARTESIAN_POINT('Ctrl Pts',(-1.03397172011655,0.40621012607091,8.62530485816356));
#11358=CARTESIAN_POINT('Ctrl Pts',(-1.13807370548541,-0.135112100279007,
8.65157605998515));
#11359=CARTESIAN_POINT('Ctrl Pts',(-0.874200603918551,-0.810033907036799,
8.68440883732023));
#11360=CARTESIAN_POINT('Ctrl Pts',(-0.0893495425282713,-1.1880032461031,
8.72379427305056));
#11361=CARTESIAN_POINT('Ctrl Pts',(0.741691192429426,-0.931226721392334,
8.76316169471054));
#11362=CARTESIAN_POINT('Ctrl Pts',(1.17652809635137,-0.178488859217621,
8.80250720794144));
#11363=CARTESIAN_POINT('Ctrl Pts',(0.982824576300801,0.669329348618244,
8.84182661196442));
#11364=CARTESIAN_POINT('Ctrl Pts',(0.385078060730947,1.07548591500891,8.87456816417469));
#11365=CARTESIAN_POINT('Ctrl Pts',(-0.163794877304455,1.09437112850357,
8.90074393179308));
#11366=CARTESIAN_POINT('Ctrl Pts',(-0.595227163902899,0.944061642655201,
8.9225472241168));
#11367=CARTESIAN_POINT('Ctrl Pts',(-0.960030174906419,0.588294670681147,
8.94651746619086));
#11368=CARTESIAN_POINT('Ctrl Pts',(-1.12375366033643,0.0575187100594699,
8.97264926310775));
#11369=CARTESIAN_POINT('Ctrl Pts',(-1.01354227711893,-0.486285552237881,
8.99876117296623));
#11370=CARTESIAN_POINT('Ctrl Pts',(-0.65710031907676,-0.911189326968473,
9.02485391772391));
#11371=CARTESIAN_POINT('Ctrl Pts',(-0.141413823150027,-1.11332884259046,
9.05092443890678));
#11372=CARTESIAN_POINT('Ctrl Pts',(0.36230898904362,-1.05015688586155,9.0748027078103));
#11373=CARTESIAN_POINT('Ctrl Pts',(0.746453838137557,-0.807699772902029,
9.09649267546183));
#11374=CARTESIAN_POINT('Ctrl Pts',(1.07231758997464,-0.369824731298935,
9.12250252624746));
#11375=CARTESIAN_POINT('Ctrl Pts',(1.12732730366444,0.345001885129974,9.15497914731887));
#11376=CARTESIAN_POINT('Ctrl Pts',(0.678756713757859,0.904746517993574,
9.18740855014101));
#11377=CARTESIAN_POINT('Ctrl Pts',(0.165507019098447,1.08244751652205,9.21331839979818));
#11378=CARTESIAN_POINT('Ctrl Pts',(-0.308999581863406,1.06560418820654,
9.23597081782354));
#11379=CARTESIAN_POINT('Ctrl Pts',(-0.794117710088271,0.797513049435794,
9.26183226756409));
#11380=CARTESIAN_POINT('Ctrl Pts',(-1.09507393875302,0.252625058546865,
9.29088748480864));
#11381=CARTESIAN_POINT('Ctrl Pts',(-1.06021949391649,-0.368467310983676,
9.31990238809889));
#11382=CARTESIAN_POINT('Ctrl Pts',(-0.767155367175566,-0.780323412962235,
9.34351106352889));
#11383=CARTESIAN_POINT('Ctrl Pts',(-0.368167386477954,-1.02413220651149,
9.36602115249684));
#11384=CARTESIAN_POINT('Ctrl Pts',(0.0348719585901695,-1.09533669341058,
9.38529619984537));
#11385=CARTESIAN_POINT('Ctrl Pts',(0.468219703484827,-0.978655860325924,
9.40668812759201));
#11386=CARTESIAN_POINT('Ctrl Pts',(0.792553898291587,-0.739500371751133,
9.42591990841105));
#11387=CARTESIAN_POINT('Ctrl Pts',(1.00681767370294,-0.398335671185081,
9.44513223986786));
#11388=CARTESIAN_POINT('Ctrl Pts',(1.07533028922252,-0.0359819011052655,
9.46272410868506));
#11389=CARTESIAN_POINT('Ctrl Pts',(1.0286539815297,0.293056390755808,9.47870105477657));
#11390=CARTESIAN_POINT('Ctrl Pts',(0.86625698295483,0.657104215112349,9.49785707208013));
#11391=CARTESIAN_POINT('Ctrl Pts',(0.484475150056015,0.998571613108099,
9.52177366135875));
#11392=CARTESIAN_POINT('Ctrl Pts',(-0.121083850117737,1.10130133263869,
9.55042230310675));
#11393=CARTESIAN_POINT('Ctrl Pts',(-0.592522878860891,0.905583663059082,
9.57425486906399));
#11394=CARTESIAN_POINT('Ctrl Pts',(-0.864209344596109,0.617325533939084,
9.59329337909015));
#11395=CARTESIAN_POINT('Ctrl Pts',(-1.04634541117236,0.265991724838279,
9.6123144658592));
#11396=CARTESIAN_POINT('Ctrl Pts',(-1.07500987210398,-0.24188060268642,
9.63605956488873));
#11397=CARTESIAN_POINT('Ctrl Pts',(-0.779954867934298,-0.775246119869282,
9.66449897772344));
#11398=CARTESIAN_POINT('Ctrl Pts',(-0.247592524130115,-1.06928473269863,
9.69288403823075));
#11399=CARTESIAN_POINT('Ctrl Pts',(0.358514842778508,-1.03509158560357,
9.72121339508318));
#11400=CARTESIAN_POINT('Ctrl Pts',(0.852503408868504,-0.684360220801713,
9.74948648590963));
#11401=CARTESIAN_POINT('Ctrl Pts',(1.08371728012903,-0.125699851986608,
9.77770245803913));
#11402=CARTESIAN_POINT('Ctrl Pts',(0.98247853245713,0.469127299242737,9.80586062858382));
#11403=CARTESIAN_POINT('Ctrl Pts',(0.581095418885572,0.917982863355751,
9.8339603391256));
#11404=CARTESIAN_POINT('Ctrl Pts',(0.00371945698538958,1.0841505904603,
9.86200090585858));
#11405=CARTESIAN_POINT('Ctrl Pts',(-0.572497970703721,0.918009674239079,
9.88998191493704));
#11406=CARTESIAN_POINT('Ctrl Pts',(-0.956015873607097,0.48830415267755,
9.91686840080534));
#11407=CARTESIAN_POINT('Ctrl Pts',(-1.06443510009297,-0.0492810426968473,
9.94266804966375));
#11408=CARTESIAN_POINT('Ctrl Pts',(-0.909357052100821,-0.550964155960349,
9.96738574321015));
#11409=CARTESIAN_POINT('Ctrl Pts',(-0.565311440336517,-0.886619648503672,
9.98999909150709));
#11410=CARTESIAN_POINT('Ctrl Pts',(-0.159295255073405,-1.02784076843099,
10.0105219760513));
#11411=CARTESIAN_POINT('Ctrl Pts',(0.356531087367818,-1.00994129487403,
10.0351110691776));
#11412=CARTESIAN_POINT('Ctrl Pts',(0.803815564251162,-0.70612787785747,
10.0596470195591));
#11413=CARTESIAN_POINT('Ctrl Pts',(1.00725255818897,-0.23415518199599,10.0841256738831));
#11414=CARTESIAN_POINT('Ctrl Pts',(1.02807331078756,0.277760194562661,10.1085663359638));
#11415=CARTESIAN_POINT('Ctrl Pts',(0.692177038145714,0.86105028376297,10.1390509198933));
#11416=CARTESIAN_POINT('Ctrl Pts',(-0.079207548479385,1.09839920332005,
10.1755177213482));
#11417=CARTESIAN_POINT('Ctrl Pts',(-0.720878115552071,0.787669451110676,
10.2078339278888));
#11418=CARTESIAN_POINT('Ctrl Pts',(-1.00668116603609,0.260095185285768,
10.2360361718044));
#11419=CARTESIAN_POINT('Ctrl Pts',(-1.00648111171243,-0.252125402489005,
10.260158097259));
#11420=CARTESIAN_POINT('Ctrl Pts',(-0.761884595208099,-0.70166277460692,
10.2842305712202));
#11421=CARTESIAN_POINT('Ctrl Pts',(-0.332829534430515,-0.978326527256894,
10.3082539354471));
#11422=CARTESIAN_POINT('Ctrl Pts',(0.175201126514412,-1.01615194386632,
10.3322257202373));
#11423=CARTESIAN_POINT('Ctrl Pts',(0.570912684782833,-0.837348131381933,
10.3526616834307));
#11424=CARTESIAN_POINT('Ctrl Pts',(0.812372874444947,-0.581335050023905,
10.3695793154414));
#11425=CARTESIAN_POINT('Ctrl Pts',(0.983676116433903,-0.250820913163252,
10.3874712603802));
#11426=CARTESIAN_POINT('Ctrl Pts',(1.01061901534878,0.226684592654012,10.4097995269886));
#11427=CARTESIAN_POINT('Ctrl Pts',(0.733269268835352,0.72798038254435,10.4365300469703));
#11428=CARTESIAN_POINT('Ctrl Pts',(0.233093165855876,1.00419866522971,10.4631992375404));
#11429=CARTESIAN_POINT('Ctrl Pts',(-0.336165877643461,0.972059073620533,
10.4898068448759));
#11430=CARTESIAN_POINT('Ctrl Pts',(-0.799969685254342,0.642727140263,10.5163536740842));
#11431=CARTESIAN_POINT('Ctrl Pts',(-1.01699704815844,0.118312035325428,
10.5428401065924));
#11432=CARTESIAN_POINT('Ctrl Pts',(-0.92196271867631,-0.439928903735246,
10.5692667693717));
#11433=CARTESIAN_POINT('Ctrl Pts',(-0.545343903600284,-0.86109976629844,
10.5956342393924));
#11434=CARTESIAN_POINT('Ctrl Pts',(-0.00357983942734503,-1.01699776973905,
10.6219431694178));
#11435=CARTESIAN_POINT('Ctrl Pts',(0.536895859987019,-0.861110061278634,
10.6481942447077));
#11436=CARTESIAN_POINT('Ctrl Pts',(0.910778345211294,-0.442480419813451,
10.6743881916688));
#11437=CARTESIAN_POINT('Ctrl Pts',(1.00442833895634,0.109709764210513,10.7005257813949));
#11438=CARTESIAN_POINT('Ctrl Pts',(0.790397648834613,0.625987767469122,
10.7266078184931));
#11439=CARTESIAN_POINT('Ctrl Pts',(0.335451246135889,0.948585082178801,
10.7526351610479));
#11440=CARTESIAN_POINT('Ctrl Pts',(-0.220246780266447,0.979624559336618,
10.7786086842944));
#11441=CARTESIAN_POINT('Ctrl Pts',(-0.706298501153887,0.710807550814349,
10.8045293452089));
#11442=CARTESIAN_POINT('Ctrl Pts',(-0.97430102068363,0.225561067647772,
10.8303980365973));
#11443=CARTESIAN_POINT('Ctrl Pts',(-0.943134026742999,-0.326798203428734,
10.8562159260074));
#11444=CARTESIAN_POINT('Ctrl Pts',(-0.623500527832522,-0.77708962181922,
10.8819836674486));
#11445=CARTESIAN_POINT('Ctrl Pts',(-0.114286877111302,-0.987848109921079,
10.9077031700225));
#11446=CARTESIAN_POINT('Ctrl Pts',(0.427995002062218,-0.89575880106675,
10.9333736290742));
#11447=CARTESIAN_POINT('Ctrl Pts',(0.837323125674483,-0.529580069932072,
10.9590003936702));
#11448=CARTESIAN_POINT('Ctrl Pts',(0.93834816881921,-0.179033497520655,
10.9760482739938));
#11449=CARTESIAN_POINT('Ctrl Pts',(0.938371883484785,-0.00287492837111495,
10.9845738995199));
#11450=CARTESIAN_POINT('Ctrl Pts',(1.0224394592446,0.00362858594397732,
7.80008768273634));
#11451=CARTESIAN_POINT('Ctrl Pts',(1.02241364265261,0.19540078259054,7.80936896800732));
#11452=CARTESIAN_POINT('Ctrl Pts',(0.912365375626032,0.57748816023679,7.82794865742167));
#11453=CARTESIAN_POINT('Ctrl Pts',(0.466303723879016,0.976511784703295,
7.85587267582946));
#11454=CARTESIAN_POINT('Ctrl Pts',(-0.12473483707645,1.07692671916304,7.88385124243725));
#11455=CARTESIAN_POINT('Ctrl Pts',(-0.679785908842397,0.847195663681504,
7.91188381887182));
#11456=CARTESIAN_POINT('Ctrl Pts',(-1.02819315903746,0.356372289452735,
7.9399697564847));
#11457=CARTESIAN_POINT('Ctrl Pts',(-1.06215795437488,-0.245685199795368,
7.96810840972975));
#11458=CARTESIAN_POINT('Ctrl Pts',(-0.770066569818735,-0.774521991341539,
7.99629908755091));
#11459=CARTESIAN_POINT('Ctrl Pts',(-0.240432926725803,-1.06742485611863,
8.0245410726846));
#11460=CARTESIAN_POINT('Ctrl Pts',(0.364933771816083,-1.0335904414025,8.05283360601858));
#11461=CARTESIAN_POINT('Ctrl Pts',(0.860379085372304,-0.682247758833767,
8.08117590069636));
#11462=CARTESIAN_POINT('Ctrl Pts',(1.09335500942013,-0.120192427037716,
8.10956712720536));
#11463=CARTESIAN_POINT('Ctrl Pts',(0.991419462258226,0.480675844038809,
8.13800642480989));
#11464=CARTESIAN_POINT('Ctrl Pts',(0.584737611570177,0.935973198560486,
8.16649288404474));
#11465=CARTESIAN_POINT('Ctrl Pts',(-0.0027678196026674,1.10536381524647,
8.19502559140558));
#11466=CARTESIAN_POINT('Ctrl Pts',(-0.59133830992197,0.935988511200654,
8.22360351453493));
#11467=CARTESIAN_POINT('Ctrl Pts',(-0.984924251409923,0.495548388775854,
8.25116567700538));
#11468=CARTESIAN_POINT('Ctrl Pts',(-1.07847291175567,0.0310816574929332,
8.27345907397737));
#11469=CARTESIAN_POINT('Ctrl Pts',(-1.02459118072371,-0.273105602170713,
8.28833656227911));
#11470=CARTESIAN_POINT('Ctrl Pts',(-0.96248957961835,-0.437297739773922,
8.29684231384406));
#11471=CARTESIAN_POINT('Ctrl Pts',(-0.839511150877903,-0.670321160019251,
8.30960497566622));
#11472=CARTESIAN_POINT('Ctrl Pts',(-0.548303540985154,-0.954553814143627,
8.32876278234068));
#11473=CARTESIAN_POINT('Ctrl Pts',(-0.0248445001511764,-1.10234641140064,
8.35433996388364));
#11474=CARTESIAN_POINT('Ctrl Pts',(0.505244368626293,-0.980683310613957,
8.37994796636545));
#11475=CARTESIAN_POINT('Ctrl Pts',(0.983298938382587,-0.561102157425724,
8.40985911563777));
#11476=CARTESIAN_POINT('Ctrl Pts',(1.15306759627895,0.17600323712225,8.44409052111051));
#11477=CARTESIAN_POINT('Ctrl Pts',(0.773321078747944,0.831505957598933,
8.4783778493315));
#11478=CARTESIAN_POINT('Ctrl Pts',(0.190424898254101,1.09310862502598,8.50842107329988));
#11479=CARTESIAN_POINT('Ctrl Pts',(-0.355521415788955,1.05241611124383,
8.53419886303447));
#11480=CARTESIAN_POINT('Ctrl Pts',(-0.778104439028643,0.779408807091155,
8.55784986417128));
#11481=CARTESIAN_POINT('Ctrl Pts',(-1.01743271691609,0.397361561177328,
8.57936934857403));
#11482=CARTESIAN_POINT('Ctrl Pts',(-1.11987755001356,-0.135106308393046,
8.60521057121674));
#11483=CARTESIAN_POINT('Ctrl Pts',(-0.860210203886423,-0.799841353930079,
8.6375404134144));
#11484=CARTESIAN_POINT('Ctrl Pts',(-0.0861596556698379,-1.17290745782566,
8.67638602671966));
#11485=CARTESIAN_POINT('Ctrl Pts',(0.734967656111525,-0.919467499002295,
8.71527555952678));
#11486=CARTESIAN_POINT('Ctrl Pts',(1.16550630786582,-0.174715119235608,
8.75420591182071));
#11487=CARTESIAN_POINT('Ctrl Pts',(0.973778738558462,0.665697588208069,
8.79317445015984));
#11488=CARTESIAN_POINT('Ctrl Pts',(0.380463090672774,1.06911800335217,8.82567420440926));
#11489=CARTESIAN_POINT('Ctrl Pts',(-0.165164537359199,1.08794158438632,
8.85169301078046));
#11490=CARTESIAN_POINT('Ctrl Pts',(-0.594400866537851,0.938439198965205,
8.87338270538702));
#11491=CARTESIAN_POINT('Ctrl Pts',(-0.95773126151556,0.584213648932498,
8.89725029751952));
#11492=CARTESIAN_POINT('Ctrl Pts',(-1.12103889708631,0.055105611023825,
8.92329682233336));
#11493=CARTESIAN_POINT('Ctrl Pts',(-1.01110710742072,-0.487664602636993,
8.94935728559613));
#11494=CARTESIAN_POINT('Ctrl Pts',(-0.655055427041069,-0.91224848520086,
8.97542181862965));
#11495=CARTESIAN_POINT('Ctrl Pts',(-0.139243614128308,-1.1145127827179,
9.00149832931453));
#11496=CARTESIAN_POINT('Ctrl Pts',(0.36516306280004,-1.05133216304336,9.02540442403775));
#11497=CARTESIAN_POINT('Ctrl Pts',(0.750234379277831,-0.808326308082215,
9.04714316415924));
#11498=CARTESIAN_POINT('Ctrl Pts',(1.07716885680808,-0.36909138500367,9.07323293203551));
#11499=CARTESIAN_POINT('Ctrl Pts',(1.13264226238729,0.348905435514389,9.10585241853449));
#11500=CARTESIAN_POINT('Ctrl Pts',(0.681535489212814,0.912168559624331,
9.13846615527862));
#11501=CARTESIAN_POINT('Ctrl Pts',(0.164491157620536,1.09123311876696,9.1645653126246));
#11502=CARTESIAN_POINT('Ctrl Pts',(-0.313915065303131,1.07428767346862,
9.18740100572472));
#11503=CARTESIAN_POINT('Ctrl Pts',(-0.803557843644582,0.803817864196927,
9.21349549904032));
#11504=CARTESIAN_POINT('Ctrl Pts',(-1.10777522245362,0.253279572730345,
9.24284916045016));
#11505=CARTESIAN_POINT('Ctrl Pts',(-1.07262556922497,-0.375096829106732,
9.27219864048019));
#11506=CARTESIAN_POINT('Ctrl Pts',(-0.775849519172851,-0.792323064162487,
9.29610586960291));
#11507=CARTESIAN_POINT('Ctrl Pts',(-0.371328745506812,-1.03953633075296,
9.31892645589477));
#11508=CARTESIAN_POINT('Ctrl Pts',(0.0376304846545741,-1.11184105971114,
9.33848334826187));
#11509=CARTESIAN_POINT('Ctrl Pts',(0.477752265059943,-0.993378524589055,
9.36020520881827));
#11510=CARTESIAN_POINT('Ctrl Pts',(0.807452663693637,-0.750309094977912,
9.37975248696025));
#11511=CARTESIAN_POINT('Ctrl Pts',(1.02542831143796,-0.403287461382024,
9.3992915884546));
#11512=CARTESIAN_POINT('Ctrl Pts',(1.09520570424478,-0.0343996015918939,
9.41719819112087));
#11513=CARTESIAN_POINT('Ctrl Pts',(1.04766435799285,0.300821003164569,9.4334730419063));
#11514=CARTESIAN_POINT('Ctrl Pts',(0.882134941333648,0.671933761076852,
9.4529986725804));
#11515=CARTESIAN_POINT('Ctrl Pts',(0.492704809338165,1.0203555390095,9.4773907315634));
#11516=CARTESIAN_POINT('Ctrl Pts',(-0.125813239292152,1.12538522726572,
9.50664807519627));
#11517=CARTESIAN_POINT('Ctrl Pts',(-0.607916474994097,0.925314738520527,
9.5310110810177));
#11518=CARTESIAN_POINT('Ctrl Pts',(-0.886009132880398,0.630281874283733,
9.55049558512337));
#11519=CARTESIAN_POINT('Ctrl Pts',(-1.07254869382692,0.270488248614126,
9.56997311484588));
#11520=CARTESIAN_POINT('Ctrl Pts',(-1.10201013131539,-0.25001327256632,
9.59430238061315));
#11521=CARTESIAN_POINT('Ctrl Pts',(-0.799358428997046,-0.797323059937847,
9.62347692829483));
#11522=CARTESIAN_POINT('Ctrl Pts',(-0.252578030159201,-1.09942897214462,
9.65262644221176));
#11523=CARTESIAN_POINT('Ctrl Pts',(0.370672782655161,-1.06436218073861,
9.68175071510106));
#11524=CARTESIAN_POINT('Ctrl Pts',(0.879222485658297,-0.703403547720322,
9.71084774442572));
#11525=CARTESIAN_POINT('Ctrl Pts',(1.11755902291746,-0.12776947340514,9.73991636014012));
#11526=CARTESIAN_POINT('Ctrl Pts',(1.01322037204631,0.485811010865536,9.76895508611072));
#11527=CARTESIAN_POINT('Ctrl Pts',(0.598843742169754,0.949332890885439,
9.79796253896268));
#11528=CARTESIAN_POINT('Ctrl Pts',(0.00212031341932294,1.12116294453614,
9.82693748941955));
#11529=CARTESIAN_POINT('Ctrl Pts',(-0.594030577562524,0.949371974584455,
9.85587828377846));
#11530=CARTESIAN_POINT('Ctrl Pts',(-0.991227126988807,0.504456962371331,
9.88371366780931));
#11531=CARTESIAN_POINT('Ctrl Pts',(-1.10366008874695,-0.0526856529500433,
9.91044589924098));
#11532=CARTESIAN_POINT('Ctrl Pts',(-0.942838790043787,-0.573096610903901,
9.93608238452499));
#11533=CARTESIAN_POINT('Ctrl Pts',(-0.585724594591535,-0.921582228722216,
9.95955452943091));
#11534=CARTESIAN_POINT('Ctrl Pts',(-0.163975590932816,-1.06829755406478,
9.98086822993116));
#11535=CARTESIAN_POINT('Ctrl Pts',(0.372168170774437,-1.04971711604162,
10.0064236491231));
#11536=CARTESIAN_POINT('Ctrl Pts',(0.837477772259037,-0.733785381710125,
10.0319384111643));
#11537=CARTESIAN_POINT('Ctrl Pts',(1.049292306327,-0.242423951232681,10.0574181798459));
#11538=CARTESIAN_POINT('Ctrl Pts',(1.0710034914769,0.29080545818794,10.0828736616323));
#11539=CARTESIAN_POINT('Ctrl Pts',(0.72099131572971,0.89885340658251,10.1146376758435));
#11540=CARTESIAN_POINT('Ctrl Pts',(-0.0838294263341789,1.14666175739243,
10.1526781887287));
#11541=CARTESIAN_POINT('Ctrl Pts',(-0.753997956341837,0.822259906126611,
10.1864162007806));
#11542=CARTESIAN_POINT('Ctrl Pts',(-1.05275079101018,0.270909471727262,
10.2158844277476));
#11543=CARTESIAN_POINT('Ctrl Pts',(-1.05256683050461,-0.26474101391336,
10.2411067512839));
#11544=CARTESIAN_POINT('Ctrl Pts',(-0.796701237850394,-0.735095856462346,
10.2662893641572));
#11545=CARTESIAN_POINT('Ctrl Pts',(-0.34759897431464,-1.02472783459927,
10.2914312125966));
#11546=CARTESIAN_POINT('Ctrl Pts',(0.18447326483658,-1.06437052854044,10.3165357251281));
#11547=CARTESIAN_POINT('Ctrl Pts',(0.599067458247316,-0.877055322325079,
10.3379407915222));
#11548=CARTESIAN_POINT('Ctrl Pts',(0.852159422370925,-0.608714393671463,
10.3556713883906));
#11549=CARTESIAN_POINT('Ctrl Pts',(1.03175866217658,-0.262202962400976,
10.3744275198819));
#11550=CARTESIAN_POINT('Ctrl Pts',(1.06003703932392,0.238542818252046,10.3978364643517));
#11551=CARTESIAN_POINT('Ctrl Pts',(0.769079304176225,0.764498896052599,
10.4258758659065));
#11552=CARTESIAN_POINT('Ctrl Pts',(0.244120099803413,1.05442656731387,10.4538609075553));
#11553=CARTESIAN_POINT('Ctrl Pts',(-0.353571270507426,1.02070521861313,
10.4817919929746));
#11554=CARTESIAN_POINT('Ctrl Pts',(-0.840707898088968,0.67483086915919,
10.5096681144061));
#11555=CARTESIAN_POINT('Ctrl Pts',(-1.06872999263526,0.123899612590722,
10.5374889758409));
#11556=CARTESIAN_POINT('Ctrl Pts',(-0.968881292507578,-0.462723739670875,
10.5652540330952));
#11557=CARTESIAN_POINT('Ctrl Pts',(-0.573043307192763,-0.905408458289749,
10.5929629214798));
#11558=CARTESIAN_POINT('Ctrl Pts',(-0.00352082082609249,-1.06930551127307,
10.6206152641652));
#11559=CARTESIAN_POINT('Ctrl Pts',(0.564731071947371,-0.90541400189164,
10.6482107513056));
#11560=CARTESIAN_POINT('Ctrl Pts',(0.957869636830534,-0.465229288689372,
10.675749107199));
#11561=CARTESIAN_POINT('Ctrl Pts',(1.05634881760394,0.115433979910032,10.7032301036035));
#11562=CARTESIAN_POINT('Ctrl Pts',(0.83127262512651,0.658347260291639,10.7306535506042));
#11563=CARTESIAN_POINT('Ctrl Pts',(0.352855070853646,0.997579943766369,
10.7580193078072));
#11564=CARTESIAN_POINT('Ctrl Pts',(-0.231480179248419,1.03021016071997,
10.7853272583561));
#11565=CARTESIAN_POINT('Ctrl Pts',(-0.742529937572376,0.747555014282395,
10.8125773674657));
#11566=CARTESIAN_POINT('Ctrl Pts',(-1.02427277250167,0.237405701771815,
10.8397695463441));
#11567=CARTESIAN_POINT('Ctrl Pts',(-0.991498148688415,-0.343196952014676,
10.8669039522539));
#11568=CARTESIAN_POINT('Ctrl Pts',(-0.655579551142097,-0.81640152144281,
10.8939803118662));
#11569=CARTESIAN_POINT('Ctrl Pts',(-0.120565700495315,-1.03781837274451,
10.9209994211754));
#11570=CARTESIAN_POINT('Ctrl Pts',(0.44900506988111,-0.941049432983352,
10.9479597810765));
#11571=CARTESIAN_POINT('Ctrl Pts',(0.878779001046494,-0.556545520129311,
10.9748651152608));
#11572=CARTESIAN_POINT('Ctrl Pts',(0.984764947260803,-0.188518733496692,
10.9927592993211));
#11573=CARTESIAN_POINT('Ctrl Pts',(0.984789826393123,-0.00371020912213119,
11.0017035606219));
#11574=CARTESIAN_POINT('Ctrl Pts',(0.999999511922295,0.00362556505265694,
7.80008768273634));
#11575=CARTESIAN_POINT('Ctrl Pts',(0.999974254701651,0.191242609375982,
7.80916786923111));
#11576=CARTESIAN_POINT('Ctrl Pts',(0.892341067491657,0.564938782877452,
7.82733932423682));
#11577=CARTESIAN_POINT('Ctrl Pts',(0.456009237357814,0.955278731473674,
7.85465504855182));
#11578=CARTESIAN_POINT('Ctrl Pts',(-0.122182810478375,1.05350592491678,
7.88202502929242));
#11579=CARTESIAN_POINT('Ctrl Pts',(-0.665220911419956,0.828753483606749,
7.90945086692426));
#11580=CARTESIAN_POINT('Ctrl Pts',(-1.00612665101876,0.348504727673495,
7.93693161942117));
#11581=CARTESIAN_POINT('Ctrl Pts',(-1.03937057711115,-0.24065277058934,
7.96446742990799));
#11582=CARTESIAN_POINT('Ctrl Pts',(-0.753506480379588,-0.758233234780652,
7.99205790686499));
#11583=CARTESIAN_POINT('Ctrl Pts',(-0.23507859765888,-1.04495072049649,
8.01970284677932));
#11584=CARTESIAN_POINT('Ctrl Pts',(0.357583215672993,-1.01183827364816,
8.04740190675199));
#11585=CARTESIAN_POINT('Ctrl Pts',(0.842723866190013,-0.667819008067397,
8.07515475263842));
#11586=CARTESIAN_POINT('Ctrl Pts',(1.07090748459127,-0.117361728527591,
8.1029609908626));
#11587=CARTESIAN_POINT('Ctrl Pts',(0.971068313490196,0.471237645030074,
8.13082019638131));
#11588=CARTESIAN_POINT('Ctrl Pts',(0.572615291983895,0.917345600069376,
8.15873190469605));
#11589=CARTESIAN_POINT('Ctrl Pts',(-0.00315068596155565,1.08336827030711,
8.18669561143439));
#11590=CARTESIAN_POINT('Ctrl Pts',(-0.580114085036881,0.917350780124834,
8.21471077684478));
#11591=CARTESIAN_POINT('Ctrl Pts',(-0.966051395769627,0.48549839913134,
8.24173733490367));
#11592=CARTESIAN_POINT('Ctrl Pts',(-1.05781582749726,0.0299567596628159,
8.2636033984339));
#11593=CARTESIAN_POINT('Ctrl Pts',(-1.00496213983024,-0.268439331682945,
8.27819794787177));
#11594=CARTESIAN_POINT('Ctrl Pts',(-0.94403781713285,-0.429519542479439,
8.28654256698954));
#11595=CARTESIAN_POINT('Ctrl Pts',(-0.823382078993268,-0.658140969899007,
8.29906435736913));
#11596=CARTESIAN_POINT('Ctrl Pts',(-0.537625296367964,-0.93706913925231,
8.31786521711992));
#11597=CARTESIAN_POINT('Ctrl Pts',(-0.0238288726443125,-1.08214769701979,
8.34297130007593));
#11598=CARTESIAN_POINT('Ctrl Pts',(0.496636287796273,-0.96271505408145,
8.36811512451513));
#11599=CARTESIAN_POINT('Ctrl Pts',(0.966152438091784,-0.550650417462692,
8.39749297986939));
#11600=CARTESIAN_POINT('Ctrl Pts',(1.13301488484768,0.17354695961988,8.43112871623582));
#11601=CARTESIAN_POINT('Ctrl Pts',(0.759782029367692,0.81792928250629,8.46483592073065));
#11602=CARTESIAN_POINT('Ctrl Pts',(0.18659690053678,1.07520238454981,8.49438045894607));
#11603=CARTESIAN_POINT('Ctrl Pts',(-0.350443601960556,1.03519669411318,
8.51973848476555));
#11604=CARTESIAN_POINT('Ctrl Pts',(-0.766297161890012,0.766560498033478,
8.54301401492018));
#11605=CARTESIAN_POINT('Ctrl Pts',(-1.00188555557132,0.390501874334262,
8.56419748306598));
#11606=CARTESIAN_POINT('Ctrl Pts',(-1.10276576842174,-0.133757727725488,
8.5896418232172));
#11607=CARTESIAN_POINT('Ctrl Pts',(-0.847050948528023,-0.7885712029239,
8.6214918164511));
#11608=CARTESIAN_POINT('Ctrl Pts',(-0.0842079511184448,-1.15633714773807,
8.65978061793639));
#11609=CARTESIAN_POINT('Ctrl Pts',(0.72557322963091,-0.906499072035091,
8.69813561803015));
#11610=CARTESIAN_POINT('Ctrl Pts',(1.15047751535783,-0.171671665185466,
8.73655413319947));
#11611=CARTESIAN_POINT('Ctrl Pts',(0.961273159473049,0.658124915791643,
8.77503338584849));
#11612=CARTESIAN_POINT('Ctrl Pts',(0.375126711265494,1.05675920723847,8.80714766479813));
#11613=CARTESIAN_POINT('Ctrl Pts',(-0.164183045710825,1.07538023554299,
8.8328665668906));
#11614=CARTESIAN_POINT('Ctrl Pts',(-0.588587403918608,0.927569264768944,
8.85431383603483));
#11615=CARTESIAN_POINT('Ctrl Pts',(-0.947989492545562,0.577208917394653,
8.87792434906622));
#11616=CARTESIAN_POINT('Ctrl Pts',(-1.10961450093061,0.0536146968196933,
8.90370345540594));
#11617=CARTESIAN_POINT('Ctrl Pts',(-1.00082022593385,-0.483727092204472,
8.92950382341385));
#11618=CARTESIAN_POINT('Ctrl Pts',(-0.648169490504554,-0.904286310022195,
8.95532452406706));
#11619=CARTESIAN_POINT('Ctrl Pts',(-0.137073525470092,-1.1047399934849,
8.98116461266558));
#11620=CARTESIAN_POINT('Ctrl Pts',(0.362995552358674,-1.04213062048012,
9.0048682588092));
#11621=CARTESIAN_POINT('Ctrl Pts',(0.744903368537152,-0.801138176501351,
9.02642976126975));
#11622=CARTESIAN_POINT('Ctrl Pts',(1.06927029269131,-0.365389501861442,
9.05231612054031));
#11623=CARTESIAN_POINT('Ctrl Pts',(1.12442623960627,0.347295239484755,9.08469656290588));
#11624=CARTESIAN_POINT('Ctrl Pts',(0.676375081319218,0.906916376424927,
9.11710422215215));
#11625=CARTESIAN_POINT('Ctrl Pts',(0.162505682592346,1.08489901523682,9.14304497362832));
#11626=CARTESIAN_POINT('Ctrl Pts',(-0.313134592199748,1.06806757295122,
9.16575116654966));
#11627=CARTESIAN_POINT('Ctrl Pts',(-0.80020652042605,0.79906113083438,9.19171186155256));
#11628=CARTESIAN_POINT('Ctrl Pts',(-1.1030130064212,0.251155630516143,9.22093071361268));
#11629=CARTESIAN_POINT('Ctrl Pts',(-1.06806000491819,-0.374587327913118,
9.25016115867103));
#11630=CARTESIAN_POINT('Ctrl Pts',(-0.772382685892504,-0.790331103336901,
9.27398680631869));
#11631=CARTESIAN_POINT('Ctrl Pts',(-0.369190625906315,-1.03674084848642,
9.29673431868371));
#11632=CARTESIAN_POINT('Ctrl Pts',(0.038576143908095,-1.10885924555696,
9.31623572825941));
#11633=CARTESIAN_POINT('Ctrl Pts',(0.477637122556786,-0.990697811322314,
9.33790778885712));
#11634=CARTESIAN_POINT('Ctrl Pts',(0.806650901305872,-0.74814670656117,
9.35741515109002));
#11635=CARTESIAN_POINT('Ctrl Pts',(1.02427838601106,-0.401712335365787,
9.37692457700679));
#11636=CARTESIAN_POINT('Ctrl Pts',(1.0939769734331,-0.0333100781542004,
9.39480970049716));
#11637=CARTESIAN_POINT('Ctrl Pts',(1.04649131988823,0.301575311206996,9.4110697587252));
#11638=CARTESIAN_POINT('Ctrl Pts',(0.881091959620118,0.67241835967004,9.43058245602211));
#11639=CARTESIAN_POINT('Ctrl Pts',(0.491781434765328,1.02078793932956,9.45497403322699));
#11640=CARTESIAN_POINT('Ctrl Pts',(-0.12690622562046,1.12590240218231,9.48424354952418));
#11641=CARTESIAN_POINT('Ctrl Pts',(-0.609455917268022,0.925702271760676,
9.50863324396813));
#11642=CARTESIAN_POINT('Ctrl Pts',(-0.887901221690915,0.630308788370616,
9.52814330365954));
#11643=CARTESIAN_POINT('Ctrl Pts',(-1.07473168029324,0.269973249594665,
9.54765198252425));
#11644=CARTESIAN_POINT('Ctrl Pts',(-1.10429179277937,-0.251571030257534,
9.57203477138778));
#11645=CARTESIAN_POINT('Ctrl Pts',(-0.800909981683876,-0.800300061810875,
9.60128772802457));
#11646=CARTESIAN_POINT('Ctrl Pts',(-0.252449360054481,-1.10339503360944,
9.63053279474191));
#11647=CARTESIAN_POINT('Ctrl Pts',(0.373097965965379,-1.06824993186655,
9.65976848374119));
#11648=CARTESIAN_POINT('Ctrl Pts',(0.883833752107615,-0.705802685092957,
9.68899331286683));
#11649=CARTESIAN_POINT('Ctrl Pts',(1.12336062251109,-0.127424704798401,
9.71820580950298));
#11650=CARTESIAN_POINT('Ctrl Pts',(1.01851100341375,0.489451283507362,9.7474045069875));
#11651=CARTESIAN_POINT('Ctrl Pts',(0.601719134479875,0.955745657723928,
9.7765879476835));
#11652=CARTESIAN_POINT('Ctrl Pts',(0.00114764771726767,1.12873118183179,
9.80575469579441));
#11653=CARTESIAN_POINT('Ctrl Pts',(-0.599201162150444,0.955775323307818,
9.83490331154648));
#11654=CARTESIAN_POINT('Ctrl Pts',(-0.999441525170258,0.507519999720283,
9.86295352909998));
#11655=CARTESIAN_POINT('Ctrl Pts',(-1.11281367201976,-0.0541281101275826,
9.88990656850941));
#11656=CARTESIAN_POINT('Ctrl Pts',(-0.950656776962806,-0.578991698652294,
9.91576396161208));
#11657=CARTESIAN_POINT('Ctrl Pts',(-0.590339529048702,-0.930637197709755,
9.93944961788225));
#11658=CARTESIAN_POINT('Ctrl Pts',(-0.164606104863989,-1.07875415066616,
9.96096785470298));
#11659=CARTESIAN_POINT('Ctrl Pts',(0.376774813272184,-1.06001813820014,
9.98677462212391));
#11660=CARTESIAN_POINT('Ctrl Pts',(0.846936223245377,-0.740877146125449,
10.0125579187175));
#11661=CARTESIAN_POINT('Ctrl Pts',(1.06107082068352,-0.244205647020787,
10.0383162020965));
#11662=CARTESIAN_POINT('Ctrl Pts',(1.08304241869915,0.294959566025181,10.0640572896683));
#11663=CARTESIAN_POINT('Ctrl Pts',(0.729014765427379,0.91016891175548,10.0962004771028));
#11664=CARTESIAN_POINT('Ctrl Pts',(-0.0857101331349617,1.16113591721249,
10.1347162317012));
#11665=CARTESIAN_POINT('Ctrl Pts',(-0.764643776951617,0.832591967114145,
10.1689000478027));
#11666=CARTESIAN_POINT('Ctrl Pts',(-1.0674640769428,0.273793097090764,10.1987708394967));
#11667=CARTESIAN_POINT('Ctrl Pts',(-1.06731019456222,-0.269314357950732,
10.22434609796));
#11668=CARTESIAN_POINT('Ctrl Pts',(-0.807788715964582,-0.746430097707613,
10.2498922819076));
#11669=CARTESIAN_POINT('Ctrl Pts',(-0.352065023972404,-1.04036411773073,
10.275408603128));
#11670=CARTESIAN_POINT('Ctrl Pts',(0.18806187608402,-1.08063605589285,10.3008942987819));
#11671=CARTESIAN_POINT('Ctrl Pts',(0.609132779330515,-0.890423751871434,
10.3226365334534));
#11672=CARTESIAN_POINT('Ctrl Pts',(0.866237924373777,-0.61783839929423,
10.3406489137734));
#11673=CARTESIAN_POINT('Ctrl Pts',(1.04872505851243,-0.26577216648544,10.3597071335657));
#11674=CARTESIAN_POINT('Ctrl Pts',(1.07750116603121,0.243190015038482,10.3835038803323));
#11675=CARTESIAN_POINT('Ctrl Pts',(0.781688530878207,0.777999980609408,
10.4120173608425));
#11676=CARTESIAN_POINT('Ctrl Pts',(0.247719136142376,1.07295015546241,10.4404872688827));
#11677=CARTESIAN_POINT('Ctrl Pts',(-0.360486616831365,1.03867188015668,
10.4689126947258));
#11678=CARTESIAN_POINT('Ctrl Pts',(-0.856395421979649,0.686612064758622,
10.4972927514314));
#11679=CARTESIAN_POINT('Ctrl Pts',(-1.08862861454113,0.125592182065228,
10.5256265935356));
#11680=CARTESIAN_POINT('Ctrl Pts',(-0.986944606168628,-0.472001059894419,
10.5539134034074));
#11681=CARTESIAN_POINT('Ctrl Pts',(-0.583594151562567,-0.923132799570535,
10.5821523997639));
#11682=CARTESIAN_POINT('Ctrl Pts',(-0.00304950196324622,-1.09023227406354,
10.6103428416619));
#11683=CARTESIAN_POINT('Ctrl Pts',(0.576397100829433,-0.923141572582211,
10.6384840153271));
#11684=CARTESIAN_POINT('Ctrl Pts',(0.977415745977647,-0.474174920735025,
10.666575250779));
#11685=CARTESIAN_POINT('Ctrl Pts',(1.07791854333959,0.118262177227866,10.6946159100158));
#11686=CARTESIAN_POINT('Ctrl Pts',(0.848237687346995,0.672348815808936,
10.7226053954193));
#11687=CARTESIAN_POINT('Ctrl Pts',(0.35987034323251,1.01866632704243,10.750543145368));
#11688=CARTESIAN_POINT('Ctrl Pts',(-0.23677931351889,1.05200727853759,10.7784286311663));
#11689=CARTESIAN_POINT('Ctrl Pts',(-0.758730842080508,0.763346883548158,
10.8062613781485));
#11690=CARTESIAN_POINT('Ctrl Pts',(-1.04655744183574,0.242222537004657,
10.8340409125563));
#11691=CARTESIAN_POINT('Ctrl Pts',(-1.01308793288556,-0.351003613269005,
10.8617668734456));
#11692=CARTESIAN_POINT('Ctrl Pts',(-0.669814425530371,-0.834593746223134,
10.889438771651));
#11693=CARTESIAN_POINT('Ctrl Pts',(-0.122977155730889,-1.06092281666227,
10.9170565165848));
#11694=CARTESIAN_POINT('Ctrl Pts',(0.459284142389985,-0.962004532278344,
10.9446192376113));
#11695=CARTESIAN_POINT('Ctrl Pts',(0.898703292351648,-0.568910379520766,
10.9721279252064));
#11696=CARTESIAN_POINT('Ctrl Pts',(1.0071027576084,-0.192548907318078,10.9904290025552));
#11697=CARTESIAN_POINT('Ctrl Pts',(1.00712819276269,-0.00361011030918905,
10.999573158519));
#11698=CARTESIAN_POINT('',(0.999999511922295,0.00362556505265694,7.80008768273634));
#11699=CARTESIAN_POINT('Origin',(1.,0.,7.875));
#11700=CARTESIAN_POINT('',(1.00712819276269,-0.00361011030918906,10.999573158519));
#11701=CARTESIAN_POINT('Ctrl Pts',(0.999999511922295,0.00362556505265694,
7.80008768273634));
#11702=CARTESIAN_POINT('Ctrl Pts',(0.999974254701651,0.191242609375982,
7.80916786923111));
#11703=CARTESIAN_POINT('Ctrl Pts',(0.892341067491657,0.564938782877452,
7.82733932423682));
#11704=CARTESIAN_POINT('Ctrl Pts',(0.456009237357814,0.955278731473674,
7.85465504855182));
#11705=CARTESIAN_POINT('Ctrl Pts',(-0.122182810478375,1.05350592491678,
7.88202502929242));
#11706=CARTESIAN_POINT('Ctrl Pts',(-0.665220911419956,0.828753483606749,
7.90945086692426));
#11707=CARTESIAN_POINT('Ctrl Pts',(-1.00612665101876,0.348504727673495,
7.93693161942117));
#11708=CARTESIAN_POINT('Ctrl Pts',(-1.03937057711115,-0.24065277058934,
7.96446742990799));
#11709=CARTESIAN_POINT('Ctrl Pts',(-0.753506480379588,-0.758233234780652,
7.99205790686499));
#11710=CARTESIAN_POINT('Ctrl Pts',(-0.23507859765888,-1.04495072049649,
8.01970284677932));
#11711=CARTESIAN_POINT('Ctrl Pts',(0.357583215672993,-1.01183827364816,
8.04740190675199));
#11712=CARTESIAN_POINT('Ctrl Pts',(0.842723866190013,-0.667819008067397,
8.07515475263842));
#11713=CARTESIAN_POINT('Ctrl Pts',(1.07090748459127,-0.117361728527591,
8.1029609908626));
#11714=CARTESIAN_POINT('Ctrl Pts',(0.971068313490196,0.471237645030074,
8.13082019638131));
#11715=CARTESIAN_POINT('Ctrl Pts',(0.572615291983895,0.917345600069376,
8.15873190469605));
#11716=CARTESIAN_POINT('Ctrl Pts',(-0.00315068596155565,1.08336827030711,
8.18669561143439));
#11717=CARTESIAN_POINT('Ctrl Pts',(-0.580114085036881,0.917350780124834,
8.21471077684478));
#11718=CARTESIAN_POINT('Ctrl Pts',(-0.966051395769627,0.48549839913134,
8.24173733490367));
#11719=CARTESIAN_POINT('Ctrl Pts',(-1.05781582749726,0.0299567596628159,
8.2636033984339));
#11720=CARTESIAN_POINT('Ctrl Pts',(-1.00496213983024,-0.268439331682945,
8.27819794787177));
#11721=CARTESIAN_POINT('Ctrl Pts',(-0.94403781713285,-0.429519542479439,
8.28654256698954));
#11722=CARTESIAN_POINT('Ctrl Pts',(-0.823382078993268,-0.658140969899007,
8.29906435736913));
#11723=CARTESIAN_POINT('Ctrl Pts',(-0.537625296367964,-0.93706913925231,
8.31786521711992));
#11724=CARTESIAN_POINT('Ctrl Pts',(-0.0238288726443125,-1.08214769701979,
8.34297130007593));
#11725=CARTESIAN_POINT('Ctrl Pts',(0.496636287796273,-0.96271505408145,
8.36811512451513));
#11726=CARTESIAN_POINT('Ctrl Pts',(0.966152438091784,-0.550650417462692,
8.39749297986939));
#11727=CARTESIAN_POINT('Ctrl Pts',(1.13301488484768,0.17354695961988,8.43112871623582));
#11728=CARTESIAN_POINT('Ctrl Pts',(0.759782029367692,0.81792928250629,8.46483592073065));
#11729=CARTESIAN_POINT('Ctrl Pts',(0.18659690053678,1.07520238454981,8.49438045894607));
#11730=CARTESIAN_POINT('Ctrl Pts',(-0.350443601960556,1.03519669411318,
8.51973848476555));
#11731=CARTESIAN_POINT('Ctrl Pts',(-0.766297161890012,0.766560498033478,
8.54301401492018));
#11732=CARTESIAN_POINT('Ctrl Pts',(-1.00188555557132,0.390501874334262,
8.56419748306598));
#11733=CARTESIAN_POINT('Ctrl Pts',(-1.10276576842174,-0.133757727725488,
8.5896418232172));
#11734=CARTESIAN_POINT('Ctrl Pts',(-0.847050948528023,-0.7885712029239,
8.6214918164511));
#11735=CARTESIAN_POINT('Ctrl Pts',(-0.0842079511184448,-1.15633714773807,
8.65978061793639));
#11736=CARTESIAN_POINT('Ctrl Pts',(0.72557322963091,-0.906499072035091,
8.69813561803015));
#11737=CARTESIAN_POINT('Ctrl Pts',(1.15047751535783,-0.171671665185466,
8.73655413319947));
#11738=CARTESIAN_POINT('Ctrl Pts',(0.961273159473049,0.658124915791643,
8.77503338584849));
#11739=CARTESIAN_POINT('Ctrl Pts',(0.375126711265494,1.05675920723847,8.80714766479813));
#11740=CARTESIAN_POINT('Ctrl Pts',(-0.164183045710825,1.07538023554299,
8.8328665668906));
#11741=CARTESIAN_POINT('Ctrl Pts',(-0.588587403918608,0.927569264768944,
8.85431383603483));
#11742=CARTESIAN_POINT('Ctrl Pts',(-0.947989492545562,0.577208917394653,
8.87792434906622));
#11743=CARTESIAN_POINT('Ctrl Pts',(-1.10961450093061,0.0536146968196933,
8.90370345540594));
#11744=CARTESIAN_POINT('Ctrl Pts',(-1.00082022593385,-0.483727092204472,
8.92950382341385));
#11745=CARTESIAN_POINT('Ctrl Pts',(-0.648169490504554,-0.904286310022195,
8.95532452406706));
#11746=CARTESIAN_POINT('Ctrl Pts',(-0.137073525470092,-1.1047399934849,
8.98116461266558));
#11747=CARTESIAN_POINT('Ctrl Pts',(0.362995552358674,-1.04213062048012,
9.0048682588092));
#11748=CARTESIAN_POINT('Ctrl Pts',(0.744903368537152,-0.801138176501351,
9.02642976126975));
#11749=CARTESIAN_POINT('Ctrl Pts',(1.06927029269131,-0.365389501861442,
9.05231612054031));
#11750=CARTESIAN_POINT('Ctrl Pts',(1.12442623960627,0.347295239484755,9.08469656290588));
#11751=CARTESIAN_POINT('Ctrl Pts',(0.676375081319218,0.906916376424927,
9.11710422215215));
#11752=CARTESIAN_POINT('Ctrl Pts',(0.162505682592346,1.08489901523682,9.14304497362832));
#11753=CARTESIAN_POINT('Ctrl Pts',(-0.313134592199748,1.06806757295122,
9.16575116654966));
#11754=CARTESIAN_POINT('Ctrl Pts',(-0.80020652042605,0.79906113083438,9.19171186155256));
#11755=CARTESIAN_POINT('Ctrl Pts',(-1.1030130064212,0.251155630516143,9.22093071361268));
#11756=CARTESIAN_POINT('Ctrl Pts',(-1.06806000491819,-0.374587327913118,
9.25016115867103));
#11757=CARTESIAN_POINT('Ctrl Pts',(-0.772382685892504,-0.790331103336901,
9.27398680631869));
#11758=CARTESIAN_POINT('Ctrl Pts',(-0.369190625906315,-1.03674084848642,
9.29673431868371));
#11759=CARTESIAN_POINT('Ctrl Pts',(0.038576143908095,-1.10885924555696,
9.31623572825941));
#11760=CARTESIAN_POINT('Ctrl Pts',(0.477637122556786,-0.990697811322314,
9.33790778885712));
#11761=CARTESIAN_POINT('Ctrl Pts',(0.806650901305872,-0.74814670656117,
9.35741515109002));
#11762=CARTESIAN_POINT('Ctrl Pts',(1.02427838601106,-0.401712335365787,
9.37692457700679));
#11763=CARTESIAN_POINT('Ctrl Pts',(1.0939769734331,-0.0333100781542004,
9.39480970049716));
#11764=CARTESIAN_POINT('Ctrl Pts',(1.04649131988823,0.301575311206996,9.4110697587252));
#11765=CARTESIAN_POINT('Ctrl Pts',(0.881091959620118,0.67241835967004,9.43058245602211));
#11766=CARTESIAN_POINT('Ctrl Pts',(0.491781434765328,1.02078793932956,9.45497403322699));
#11767=CARTESIAN_POINT('Ctrl Pts',(-0.12690622562046,1.12590240218231,9.48424354952418));
#11768=CARTESIAN_POINT('Ctrl Pts',(-0.609455917268022,0.925702271760676,
9.50863324396813));
#11769=CARTESIAN_POINT('Ctrl Pts',(-0.887901221690915,0.630308788370616,
9.52814330365954));
#11770=CARTESIAN_POINT('Ctrl Pts',(-1.07473168029324,0.269973249594665,
9.54765198252425));
#11771=CARTESIAN_POINT('Ctrl Pts',(-1.10429179277937,-0.251571030257534,
9.57203477138778));
#11772=CARTESIAN_POINT('Ctrl Pts',(-0.800909981683876,-0.800300061810875,
9.60128772802457));
#11773=CARTESIAN_POINT('Ctrl Pts',(-0.252449360054481,-1.10339503360944,
9.63053279474191));
#11774=CARTESIAN_POINT('Ctrl Pts',(0.373097965965379,-1.06824993186655,
9.65976848374119));
#11775=CARTESIAN_POINT('Ctrl Pts',(0.883833752107615,-0.705802685092957,
9.68899331286683));
#11776=CARTESIAN_POINT('Ctrl Pts',(1.12336062251109,-0.127424704798401,
9.71820580950298));
#11777=CARTESIAN_POINT('Ctrl Pts',(1.01851100341375,0.489451283507362,9.7474045069875));
#11778=CARTESIAN_POINT('Ctrl Pts',(0.601719134479875,0.955745657723928,
9.7765879476835));
#11779=CARTESIAN_POINT('Ctrl Pts',(0.00114764771726767,1.12873118183179,
9.80575469579441));
#11780=CARTESIAN_POINT('Ctrl Pts',(-0.599201162150444,0.955775323307818,
9.83490331154648));
#11781=CARTESIAN_POINT('Ctrl Pts',(-0.999441525170258,0.507519999720283,
9.86295352909998));
#11782=CARTESIAN_POINT('Ctrl Pts',(-1.11281367201976,-0.0541281101275826,
9.88990656850941));
#11783=CARTESIAN_POINT('Ctrl Pts',(-0.950656776962806,-0.578991698652294,
9.91576396161208));
#11784=CARTESIAN_POINT('Ctrl Pts',(-0.590339529048702,-0.930637197709755,
9.93944961788225));
#11785=CARTESIAN_POINT('Ctrl Pts',(-0.164606104863989,-1.07875415066616,
9.96096785470298));
#11786=CARTESIAN_POINT('Ctrl Pts',(0.376774813272184,-1.06001813820014,
9.98677462212391));
#11787=CARTESIAN_POINT('Ctrl Pts',(0.846936223245377,-0.740877146125449,
10.0125579187175));
#11788=CARTESIAN_POINT('Ctrl Pts',(1.06107082068352,-0.244205647020787,
10.0383162020965));
#11789=CARTESIAN_POINT('Ctrl Pts',(1.08304241869915,0.294959566025181,10.0640572896683));
#11790=CARTESIAN_POINT('Ctrl Pts',(0.729014765427379,0.91016891175548,10.0962004771028));
#11791=CARTESIAN_POINT('Ctrl Pts',(-0.0857101331349617,1.16113591721249,
10.1347162317012));
#11792=CARTESIAN_POINT('Ctrl Pts',(-0.764643776951617,0.832591967114145,
10.1689000478027));
#11793=CARTESIAN_POINT('Ctrl Pts',(-1.0674640769428,0.273793097090764,10.1987708394967));
#11794=CARTESIAN_POINT('Ctrl Pts',(-1.06731019456222,-0.269314357950732,
10.22434609796));
#11795=CARTESIAN_POINT('Ctrl Pts',(-0.807788715964582,-0.746430097707613,
10.2498922819076));
#11796=CARTESIAN_POINT('Ctrl Pts',(-0.352065023972404,-1.04036411773073,
10.275408603128));
#11797=CARTESIAN_POINT('Ctrl Pts',(0.18806187608402,-1.08063605589285,10.3008942987819));
#11798=CARTESIAN_POINT('Ctrl Pts',(0.609132779330515,-0.890423751871434,
10.3226365334534));
#11799=CARTESIAN_POINT('Ctrl Pts',(0.866237924373777,-0.61783839929423,
10.3406489137734));
#11800=CARTESIAN_POINT('Ctrl Pts',(1.04872505851243,-0.26577216648544,10.3597071335657));
#11801=CARTESIAN_POINT('Ctrl Pts',(1.07750116603121,0.243190015038482,10.3835038803323));
#11802=CARTESIAN_POINT('Ctrl Pts',(0.781688530878207,0.777999980609408,
10.4120173608425));
#11803=CARTESIAN_POINT('Ctrl Pts',(0.247719136142376,1.07295015546241,10.4404872688827));
#11804=CARTESIAN_POINT('Ctrl Pts',(-0.360486616831365,1.03867188015668,
10.4689126947258));
#11805=CARTESIAN_POINT('Ctrl Pts',(-0.856395421979649,0.686612064758622,
10.4972927514314));
#11806=CARTESIAN_POINT('Ctrl Pts',(-1.08862861454113,0.125592182065228,
10.5256265935356));
#11807=CARTESIAN_POINT('Ctrl Pts',(-0.986944606168628,-0.472001059894419,
10.5539134034074));
#11808=CARTESIAN_POINT('Ctrl Pts',(-0.583594151562567,-0.923132799570535,
10.5821523997639));
#11809=CARTESIAN_POINT('Ctrl Pts',(-0.00304950196324622,-1.09023227406354,
10.6103428416619));
#11810=CARTESIAN_POINT('Ctrl Pts',(0.576397100829433,-0.923141572582211,
10.6384840153271));
#11811=CARTESIAN_POINT('Ctrl Pts',(0.977415745977647,-0.474174920735025,
10.666575250779));
#11812=CARTESIAN_POINT('Ctrl Pts',(1.07791854333959,0.118262177227866,10.6946159100158));
#11813=CARTESIAN_POINT('Ctrl Pts',(0.848237687346995,0.672348815808936,
10.7226053954193));
#11814=CARTESIAN_POINT('Ctrl Pts',(0.35987034323251,1.01866632704243,10.750543145368));
#11815=CARTESIAN_POINT('Ctrl Pts',(-0.23677931351889,1.05200727853759,10.7784286311663));
#11816=CARTESIAN_POINT('Ctrl Pts',(-0.758730842080508,0.763346883548158,
10.8062613781485));
#11817=CARTESIAN_POINT('Ctrl Pts',(-1.04655744183574,0.242222537004657,
10.8340409125563));
#11818=CARTESIAN_POINT('Ctrl Pts',(-1.01308793288556,-0.351003613269005,
10.8617668734456));
#11819=CARTESIAN_POINT('Ctrl Pts',(-0.669814425530371,-0.834593746223134,
10.889438771651));
#11820=CARTESIAN_POINT('Ctrl Pts',(-0.122977155730889,-1.06092281666227,
10.9170565165848));
#11821=CARTESIAN_POINT('Ctrl Pts',(0.459284142389985,-0.962004532278344,
10.9446192376113));
#11822=CARTESIAN_POINT('Ctrl Pts',(0.898703292351648,-0.568910379520766,
10.9721279252064));
#11823=CARTESIAN_POINT('Ctrl Pts',(1.0071027576084,-0.192548907318078,10.9904290025552));
#11824=CARTESIAN_POINT('Ctrl Pts',(1.00712819276269,-0.00361011030918905,
10.999573158519));
#11825=CARTESIAN_POINT('Origin',(1.,-2.44249065417534E-15,10.925));
#11826=CARTESIAN_POINT('Origin',(1.,-2.44249065417534E-15,10.925));
#11827=CARTESIAN_POINT('Origin',(1.,0.,7.875));
#11828=CARTESIAN_POINT('',(0.,0.,0.));
#11829=CARTESIAN_POINT('',(0.,0.,0.));
#11830=CARTESIAN_POINT('Origin',(0.,0.,0.));
#11831=CARTESIAN_POINT('',(-1.070235,-0.308121667383195,-1.31065986708547E-16));
#11832=CARTESIAN_POINT('',(-1.31065986708547E-16,-0.308121667383195,1.070235));
#11833=CARTESIAN_POINT('Origin',(0.,-0.308121667383195,0.));
#11834=CARTESIAN_POINT('Origin',(0.,-0.308121667383195,0.));
#11835=CARTESIAN_POINT('',(-1.31065986708547E-16,0.308121667383195,1.070235));
#11836=CARTESIAN_POINT('Origin',(-1.34711147906209E-16,0.,1.1));
#11837=CARTESIAN_POINT('',(-1.070235,0.308121667383195,1.31065986708547E-16));
#11838=CARTESIAN_POINT('Origin',(0.,0.308121667383195,0.));
#11839=CARTESIAN_POINT('Origin',(0.,0.308121667383195,0.));
#11840=CARTESIAN_POINT('Origin',(0.,0.,0.));
#11841=CARTESIAN_POINT('',(-1.070235,0.5,-1.31065986708547E-16));
#11842=CARTESIAN_POINT('',(-1.070235,0.,-1.31065986708547E-16));
#11843=CARTESIAN_POINT('Origin',(0.,0.5,0.));
#11844=CARTESIAN_POINT('Origin',(0.,0.,0.));
#11845=CARTESIAN_POINT('',(-0.6,-0.44,-7.34788079488412E-17));
#11846=CARTESIAN_POINT('Origin',(0.,-0.44,0.));
#11847=CARTESIAN_POINT('',(-0.6,0.44,-7.34788079488412E-17));
#11848=CARTESIAN_POINT('',(-0.6,0.,-7.34788079488412E-17));
#11849=CARTESIAN_POINT('Origin',(0.,0.44,0.));
#11850=CARTESIAN_POINT('Origin',(0.,0.47,0.));
#11851=CARTESIAN_POINT('',(-0.66,0.5,-8.08266887437253E-17));
#11852=CARTESIAN_POINT('',(-0.63,0.47,-7.71527483462832E-17));
#11853=CARTESIAN_POINT('Origin',(0.,0.5,0.));
#11854=CARTESIAN_POINT('Origin',(1.070235,0.5,0.));
#11855=CARTESIAN_POINT('Origin',(0.,0.,0.));
#11856=CARTESIAN_POINT('',(-1.070235,-0.5,-1.31065986708547E-16));
#11857=CARTESIAN_POINT('Origin',(0.,-0.5,0.));
#11858=CARTESIAN_POINT('',(-1.070235,0.,-1.31065986708547E-16));
#11859=CARTESIAN_POINT('Origin',(0.66,-0.5,0.));
#11860=CARTESIAN_POINT('',(-0.66,-0.5,-8.08266887437253E-17));
#11861=CARTESIAN_POINT('Origin',(0.,-0.5,0.));
#11862=CARTESIAN_POINT('Origin',(0.,-0.47,0.));
#11863=CARTESIAN_POINT('',(-0.63,-0.47,-7.71527483462832E-17));
#11864=CARTESIAN_POINT('',(0.,0.,0.));
#11865=CARTESIAN_POINT('Origin',(0.,0.,0.));
#11866=CARTESIAN_POINT('',(-1.129765,0.308121667383195,-1.38356309103871E-16));
#11867=CARTESIAN_POINT('',(-1.38356309103871E-16,0.308121667383195,1.129765));
#11868=CARTESIAN_POINT('Origin',(0.,0.308121667383195,0.));
#11869=CARTESIAN_POINT('Origin',(0.,0.308121667383195,0.));
#11870=CARTESIAN_POINT('',(-1.38356309103871E-16,-0.308121667383195,1.129765));
#11871=CARTESIAN_POINT('Origin',(-1.34711147906209E-16,0.,1.1));
#11872=CARTESIAN_POINT('',(-1.129765,-0.308121667383195,1.38356309103871E-16));
#11873=CARTESIAN_POINT('Origin',(0.,-0.308121667383195,0.));
#11874=CARTESIAN_POINT('Origin',(0.,-0.308121667383195,0.));
#11875=CARTESIAN_POINT('Origin',(0.,0.,0.));
#11876=CARTESIAN_POINT('',(-1.129765,-0.5,-1.38356309103871E-16));
#11877=CARTESIAN_POINT('Origin',(0.,-0.5,0.));
#11878=CARTESIAN_POINT('',(-1.129765,0.,-1.38356309103871E-16));
#11879=CARTESIAN_POINT('Origin',(1.54,0.5,0.));
#11880=CARTESIAN_POINT('',(-1.54,0.5,-1.88595607068692E-16));
#11881=CARTESIAN_POINT('Origin',(0.,0.5,0.));
#11882=CARTESIAN_POINT('',(-1.129765,0.5,-1.38356309103871E-16));
#11883=CARTESIAN_POINT('Origin',(0.,0.5,0.));
#11884=CARTESIAN_POINT('Origin',(0.,0.47,0.));
#11885=CARTESIAN_POINT('',(-1.6,0.44,-1.95943487863577E-16));
#11886=CARTESIAN_POINT('Origin',(0.,0.44,0.));
#11887=CARTESIAN_POINT('',(-1.57,0.47,-1.92269547466134E-16));
#11888=CARTESIAN_POINT('Origin',(0.,0.,0.));
#11889=CARTESIAN_POINT('',(-1.6,-0.44,-1.95943487863577E-16));
#11890=CARTESIAN_POINT('Origin',(0.,-0.44,0.));
#11891=CARTESIAN_POINT('',(-1.6,0.,-1.95943487863577E-16));
#11892=CARTESIAN_POINT('Origin',(0.,-0.47,0.));
#11893=CARTESIAN_POINT('',(-1.54,-0.5,-1.88595607068692E-16));
#11894=CARTESIAN_POINT('Origin',(0.,-0.5,0.));
#11895=CARTESIAN_POINT('',(-1.57,-0.47,-1.92269547466134E-16));
#11896=CARTESIAN_POINT('Origin',(1.129765,-0.5,0.));
#11897=CARTESIAN_POINT('Origin',(0.,0.,0.));
#11898=CARTESIAN_POINT('',(-1.129765,0.,-1.38356309103871E-16));
#11899=CARTESIAN_POINT('',(0.,0.,0.));
#11900=CARTESIAN_POINT('Origin',(1.1,0.,0.));
#11901=CARTESIAN_POINT('',(1.1,-2.23201749654651E-33,0.29765));
#11902=CARTESIAN_POINT('',(1.1,-2.23201749654651E-33,-0.29765));
#11903=CARTESIAN_POINT('Origin',(1.1,0.,0.));
#11904=CARTESIAN_POINT('Origin',(0.685838782044607,0.,-0.860014630714833));
#11905=CARTESIAN_POINT('',(0.918550922801216,-5.31350540756609E-33,-0.674432891191581));
#11906=CARTESIAN_POINT('',(0.453126641287998,8.49470414473068E-34,-1.04559637023808));
#11907=CARTESIAN_POINT('Origin',(0.685838782044607,0.,-0.860014630714833));
#11908=CARTESIAN_POINT('Origin',(-0.244773027351946,0.,-1.07242070340001));
#11909=CARTESIAN_POINT('',(0.0454142657089739,-2.23201749654651E-33,-1.1386540593921));
#11910=CARTESIAN_POINT('',(-0.534960320412865,-2.23201749654651E-33,-1.00618734740791));
#11911=CARTESIAN_POINT('Origin',(-0.244773027351946,0.,-1.07242070340001));
#11912=CARTESIAN_POINT('Origin',(-0.991065754692661,0.,-0.477272113029314));
#11913=CARTESIAN_POINT('',(-0.86192025974432,8.49470414473067E-34,-0.745445496560469));
#11914=CARTESIAN_POINT('',(-1.120211249641,-5.31350540756609E-33,-0.209098729498159));
#11915=CARTESIAN_POINT('Origin',(-0.991065754692661,0.,-0.477272113029314));
#11916=CARTESIAN_POINT('Origin',(-0.991065754692661,0.,0.477272113029314));
#11917=CARTESIAN_POINT('',(-1.120211249641,-2.23201749654651E-33,0.209098729498159));
#11918=CARTESIAN_POINT('',(-0.86192025974432,-2.23201749654651E-33,0.745445496560469));
#11919=CARTESIAN_POINT('Origin',(-0.991065754692661,0.,0.477272113029314));
#11920=CARTESIAN_POINT('Origin',(-0.244773027351946,0.,1.07242070340001));
#11921=CARTESIAN_POINT('',(-0.534960320412866,-2.23201749654651E-33,1.00618734740791));
#11922=CARTESIAN_POINT('',(0.0454142657089737,-2.23201749654651E-33,1.1386540593921));
#11923=CARTESIAN_POINT('Origin',(-0.244773027351946,0.,1.07242070340001));
#11924=CARTESIAN_POINT('Origin',(0.685838782044607,0.,0.860014630714833));
#11925=CARTESIAN_POINT('',(0.453126641287998,-2.23201749654651E-33,1.04559637023808));
#11926=CARTESIAN_POINT('',(0.918550922801216,-2.23201749654651E-33,0.674432891191581));
#11927=CARTESIAN_POINT('Origin',(0.685838782044607,0.,0.860014630714833));
#11928=CARTESIAN_POINT('',(0.,0.,0.));
#11929=CARTESIAN_POINT('Origin',(0.685838782044607,0.,0.860014630714833));
#11930=CARTESIAN_POINT('',(0.413083465285518,-0.05953,0.993751811093549));
#11931=CARTESIAN_POINT('',(0.876916659919095,-0.05953,0.623857181492959));
#11932=CARTESIAN_POINT('Ctrl Pts',(0.413083465285518,-0.05953,0.993751811093549));
#11933=CARTESIAN_POINT('Ctrl Pts',(0.419070565453383,-0.0925528133349865,
0.991263089003441));
#11934=CARTESIAN_POINT('Ctrl Pts',(0.430199341854858,-0.124911173756694,
0.986608710139579));
#11935=CARTESIAN_POINT('Ctrl Pts',(0.457978755888596,-0.177924977804098,
0.973971221090534));
#11936=CARTESIAN_POINT('Ctrl Pts',(0.473077587363685,-0.199697230012983,
0.966820759530997));
#11937=CARTESIAN_POINT('Ctrl Pts',(0.507057380724533,-0.237895043532788,
0.949440676105255));
#11938=CARTESIAN_POINT('Ctrl Pts',(0.525933334162555,-0.254319232363049,
0.939198248544428));
#11939=CARTESIAN_POINT('Ctrl Pts',(0.564362943424238,-0.28018331644634,
0.916597376014514));
#11940=CARTESIAN_POINT('Ctrl Pts',(0.585840553788742,-0.29104845371857,
0.903141581680914));
#11941=CARTESIAN_POINT('Ctrl Pts',(0.629305439856167,-0.30527573347708,
0.873412008702649));
#11942=CARTESIAN_POINT('Ctrl Pts',(0.651278921914856,-0.308638795020976,
0.857118508332695));
#11943=CARTESIAN_POINT('Ctrl Pts',(0.690705563850638,-0.308638795020976,
0.825676810575914));
#11944=CARTESIAN_POINT('Ctrl Pts',(0.711480111898423,-0.30527573347708,
0.807879894508811));
#11945=CARTESIAN_POINT('Ctrl Pts',(0.750136149454208,-0.29104845371857,
0.772120216227122));
#11946=CARTESIAN_POINT('Ctrl Pts',(0.768033796848072,-0.28018331644634,
0.754175290318038));
#11947=CARTESIAN_POINT('Ctrl Pts',(0.798619410861634,-0.254319232363049,
0.721738358858166));
#11948=CARTESIAN_POINT('Ctrl Pts',(0.812805334167529,-0.237895043532788,
0.705614819529209));
#11949=CARTESIAN_POINT('Ctrl Pts',(0.837310877969633,-0.199697230012983,
0.676354402927683));
#11950=CARTESIAN_POINT('Ctrl Pts',(0.847641868610495,-0.177924977804098,
0.663225258065736));
#11951=CARTESIAN_POINT('Ctrl Pts',(0.866144010579847,-0.124911173756694,
0.638954437806245));
#11952=CARTESIAN_POINT('Ctrl Pts',(0.873158080166742,-0.0925528133349865,
0.62914037979579));
#11953=CARTESIAN_POINT('Ctrl Pts',(0.876916659919095,-0.05953,0.623857181492959));
#11954=CARTESIAN_POINT('',(0.437601487681057,-0.05953,1.03511272300331));
#11955=CARTESIAN_POINT('Origin',(0.685838782044607,-0.05953,0.860014630714833));
#11956=CARTESIAN_POINT('',(0.911784794170997,-0.05953,0.656964154625313));
#11957=CARTESIAN_POINT('Ctrl Pts',(0.911784794170998,-0.0595300000000001,
0.656964154625312));
#11958=CARTESIAN_POINT('Ctrl Pts',(0.909827729890942,-0.0762225747374255,
0.659680317203144));
#11959=CARTESIAN_POINT('Ctrl Pts',(0.907004864562642,-0.0928409665394228,
0.663576540841106));
#11960=CARTESIAN_POINT('Ctrl Pts',(0.895234408667242,-0.144299303100741,
0.679480524217551));
#11961=CARTESIAN_POINT('Ctrl Pts',(0.882797231409153,-0.177024326825049,
0.695831250979106));
#11962=CARTESIAN_POINT('Ctrl Pts',(0.854332839576145,-0.227269801620064,
0.73042219438957));
#11963=CARTESIAN_POINT('Ctrl Pts',(0.834863020612702,-0.251265615809407,
0.752807465209441));
#11964=CARTESIAN_POINT('Ctrl Pts',(0.800439809856111,-0.279889827963178,
0.789147407129766));
#11965=CARTESIAN_POINT('Ctrl Pts',(0.781998747691871,-0.290879136862659,
0.80756613568454));
#11966=CARTESIAN_POINT('Ctrl Pts',(0.742239891936898,-0.305251990234487,
0.844254137480382));
#11967=CARTESIAN_POINT('Ctrl Pts',(0.720906778729541,-0.308638795020976,
0.862505527716294));
#11968=CARTESIAN_POINT('Ctrl Pts',(0.680463863683392,-0.308638795020976,
0.894757676234429));
#11969=CARTESIAN_POINT('Ctrl Pts',(0.657923009631182,-0.305251990234488,
0.91149460735272));
#11970=CARTESIAN_POINT('Ctrl Pts',(0.613307674922609,-0.290879136862659,
0.942092777160053));
#11971=CARTESIAN_POINT('Ctrl Pts',(0.591247219971725,-0.279889827963178,
0.955972930713954));
#11972=CARTESIAN_POINT('Ctrl Pts',(0.548158511259202,-0.251265615809407,
0.981446681891443));
#11973=CARTESIAN_POINT('Ctrl Pts',(0.522002043615455,-0.227269801620063,
0.995447160474328));
#11974=CARTESIAN_POINT('Ctrl Pts',(0.481944444320713,-0.177024326825049,
1.01550068154148));
#11975=CARTESIAN_POINT('Ctrl Pts',(0.463236132117164,-0.14429930310074,
1.0239876538093));
#11976=CARTESIAN_POINT('Ctrl Pts',(0.445111721969657,-0.0928409665394226,
1.03192403056628));
#11977=CARTESIAN_POINT('Ctrl Pts',(0.440685038163619,-0.0762225747374254,
1.03380912944435));
#11978=CARTESIAN_POINT('Ctrl Pts',(0.437601487681056,-0.05953,1.03511272300331));
#11979=CARTESIAN_POINT('Origin',(0.685838782044607,-0.05953,0.860014630714833));
#11980=CARTESIAN_POINT('Origin',(0.,-0.208355,0.));
#11981=CARTESIAN_POINT('',(0.0548532617164168,-0.05953,1.12247250791415));
#11982=CARTESIAN_POINT('Origin',(0.,-0.05953,0.));
#11983=CARTESIAN_POINT('',(-0.536443649899848,-0.05953,0.987512846410683));
#11984=CARTESIAN_POINT('Ctrl Pts',(0.0548532617164173,-0.0595300000000001,
1.12247250791414));
#11985=CARTESIAN_POINT('Ctrl Pts',(0.05150947068137,-0.0762225747374254,
1.12263591311425));
#11986=CARTESIAN_POINT('Ctrl Pts',(0.0467032526342597,-0.0928409665394227,
1.12285816383385));
#11987=CARTESIAN_POINT('Ctrl Pts',(0.0269302585198975,-0.144299303100741,
1.12357162229597));
#11988=CARTESIAN_POINT('Ctrl Pts',(0.006392292392153,-0.177024326825049,
1.12404235695137));
#11989=CARTESIAN_POINT('Ctrl Pts',(-0.0383992541984087,-0.227269801620063,
1.12335509974011));
#11990=CARTESIAN_POINT('Ctrl Pts',(-0.0680399972366993,-0.251265615809407,
1.12208997038458));
#11991=CARTESIAN_POINT('Ctrl Pts',(-0.117914228755037,-0.279889827963178,
1.1178344036749));
#11992=CARTESIAN_POINT('Ctrl Pts',(-0.14381238480104,-0.290879136862659,
1.11490049012186));
#11993=CARTESIAN_POINT('Ctrl Pts',(-0.19728546073067,-0.305251990234488,
1.10669035995599));
#11994=CARTESIAN_POINT('Ctrl Pts',(-0.224855950742601,-0.308638795020976,
1.10139101611326));
#11995=CARTESIAN_POINT('Ctrl Pts',(-0.275287440920027,-0.308638795020976,
1.0898803575765));
#11996=CARTESIAN_POINT('Ctrl Pts',(-0.302426893214945,-0.305251990234488,
1.08269251410343));
#11997=CARTESIAN_POINT('Ctrl Pts',(-0.35416671187353,-0.290879136862659,
1.06688848765783));
#11998=CARTESIAN_POINT('Ctrl Pts',(-0.3787731215897,-0.279889827963178,
1.05829506364875));
#11999=CARTESIAN_POINT('Ctrl Pts',(-0.425554672694338,-0.251265615809407,
1.04048957871266));
#12000=CARTESIAN_POINT('Ctrl Pts',(-0.452808978448581,-0.227269801620063,
1.02876878445619));
#12001=CARTESIAN_POINT('Ctrl Pts',(-0.493462957200432,-0.177024326825049,
1.0099536580922));
#12002=CARTESIAN_POINT('Ctrl Pts',(-0.511762781179148,-0.14429930310074,
1.00061845128527));
#12003=CARTESIAN_POINT('Ctrl Pts',(-0.529268075276157,-0.0928409665394226,
0.991396466802468));
#12004=CARTESIAN_POINT('Ctrl Pts',(-0.533501897135713,-0.0762225747374254,
0.989110885965947));
#12005=CARTESIAN_POINT('Ctrl Pts',(-0.536443649899848,-0.0595300000000001,
0.987512846410683));
#12006=CARTESIAN_POINT('',(-0.843383895613249,-0.05953,0.742736168477219));
#12007=CARTESIAN_POINT('Origin',(0.,-0.05953,0.));
#12008=CARTESIAN_POINT('',(-1.10653577764992,-0.05953,0.196295654879792));
#12009=CARTESIAN_POINT('Ctrl Pts',(-0.843383895613249,-0.0595300000000001,
0.742736168477219));
#12010=CARTESIAN_POINT('Ctrl Pts',(-0.84559647055299,-0.0762225747374255,
0.740223768851062));
#12011=CARTESIAN_POINT('Ctrl Pts',(-0.848766861100456,-0.0928409665394227,
0.736604687327351));
#12012=CARTESIAN_POINT('Ctrl Pts',(-0.861652925570091,-0.144299303100741,
0.721590372101268));
#12013=CARTESIAN_POINT('Ctrl Pts',(-0.87482617317514,-0.177024326825049,
0.705826641853758));
#12014=CARTESIAN_POINT('Ctrl Pts',(-0.902215926359523,-0.227269801620063,
0.670378702718353));
#12015=CARTESIAN_POINT('Ctrl Pts',(-0.919707509403859,-0.251265615809407,
0.646415841396062));
#12016=CARTESIAN_POINT('Ctrl Pts',(-0.947476448101718,-0.279889827963178,
0.604769294586516));
#12017=CARTESIAN_POINT('Ctrl Pts',(-0.961329858300736,-0.290879136862659,
0.582692035672022));
#12018=CARTESIAN_POINT('Ctrl Pts',(-0.988250837578047,-0.305251990234488,
0.535766169015486));
#12019=CARTESIAN_POINT('Ctrl Pts',(-1.00129756308006,-0.308638795020976,
0.510906605094603));
#12020=CARTESIAN_POINT('Ctrl Pts',(-1.02374168767024,-0.308638795020976,
0.46430090015576));
#12021=CARTESIAN_POINT('Ctrl Pts',(-1.03504317708586,-0.305251990234488,
0.438600874831839));
#12022=CARTESIAN_POINT('Ctrl Pts',(-1.05494634094458,-0.290879136862659,
0.388295406390235));
#12023=CARTESIAN_POINT('Ctrl Pts',(-1.06356957703048,-0.279889827963178,
0.363699428370917));
#12024=CARTESIAN_POINT('Ctrl Pts',(-1.0788165083757,-0.251265615809407,
0.316022600643821));
#12025=CARTESIAN_POINT('Ctrl Pts',(-1.08664560412098,-0.227269801620063,
0.287406530683752));
#12026=CARTESIAN_POINT('Ctrl Pts',(-1.09728268713976,-0.177024326825049,
0.243890930799337));
#12027=CARTESIAN_POINT('Ctrl Pts',(-1.10139388218929,-0.144299303100741,
0.22376314604679));
#12028=CARTESIAN_POINT('Ctrl Pts',(-1.10509821673782,-0.0928409665394227,
0.204327142733961));
#12029=CARTESIAN_POINT('Ctrl Pts',(-1.10595102243643,-0.0762225747374254,
0.199591971170104));
#12030=CARTESIAN_POINT('Ctrl Pts',(-1.10653577764992,-0.0595300000000001,
0.196295654879792));
#12031=CARTESIAN_POINT('',(-1.123812,-0.05953,1.37627276864339E-16));
#12032=CARTESIAN_POINT('Origin',(0.,-0.05953,0.));
#12033=CARTESIAN_POINT('',(-1.123812,-0.35718,1.37627276864339E-16));
#12034=CARTESIAN_POINT('',(-1.123812,-0.208355,1.37627276864339E-16));
#12035=CARTESIAN_POINT('Origin',(0.,-0.35718,0.));
#12036=CARTESIAN_POINT('',(-1.10653577764992,-0.05953,-0.196295654879793));
#12037=CARTESIAN_POINT('Origin',(0.,-0.05953,0.));
#12038=CARTESIAN_POINT('',(-0.843383895613249,-0.05953,-0.742736168477219));
#12039=CARTESIAN_POINT('Ctrl Pts',(-1.10653577764992,-0.0595300000000001,
-0.196295654879792));
#12040=CARTESIAN_POINT('Ctrl Pts',(-1.10595102243643,-0.0762225747374255,
-0.199591971170104));
#12041=CARTESIAN_POINT('Ctrl Pts',(-1.10509821673782,-0.0928409665394228,
-0.204327142733962));
#12042=CARTESIAN_POINT('Ctrl Pts',(-1.10139388218929,-0.144299303100741,
-0.22376314604679));
#12043=CARTESIAN_POINT('Ctrl Pts',(-1.09728268713976,-0.177024326825049,
-0.243890930799338));
#12044=CARTESIAN_POINT('Ctrl Pts',(-1.08664560412098,-0.227269801620063,
-0.287406530683753));
#12045=CARTESIAN_POINT('Ctrl Pts',(-1.0788165083757,-0.251265615809407,
-0.316022600643821));
#12046=CARTESIAN_POINT('Ctrl Pts',(-1.06356957703048,-0.279889827963178,
-0.363699428370918));
#12047=CARTESIAN_POINT('Ctrl Pts',(-1.05494634094458,-0.290879136862659,
-0.388295406390235));
#12048=CARTESIAN_POINT('Ctrl Pts',(-1.03504317708586,-0.305251990234488,
-0.438600874831839));
#12049=CARTESIAN_POINT('Ctrl Pts',(-1.02374168767024,-0.308638795020976,
-0.46430090015576));
#12050=CARTESIAN_POINT('Ctrl Pts',(-1.00129756308006,-0.308638795020976,
-0.510906605094603));
#12051=CARTESIAN_POINT('Ctrl Pts',(-0.988250837578047,-0.305251990234488,
-0.535766169015486));
#12052=CARTESIAN_POINT('Ctrl Pts',(-0.961329858300736,-0.290879136862659,
-0.582692035672022));
#12053=CARTESIAN_POINT('Ctrl Pts',(-0.947476448101718,-0.279889827963178,
-0.604769294586516));
#12054=CARTESIAN_POINT('Ctrl Pts',(-0.919707509403859,-0.251265615809407,
-0.646415841396062));
#12055=CARTESIAN_POINT('Ctrl Pts',(-0.902215926359523,-0.227269801620064,
-0.670378702718353));
#12056=CARTESIAN_POINT('Ctrl Pts',(-0.87482617317514,-0.177024326825049,
-0.705826641853758));
#12057=CARTESIAN_POINT('Ctrl Pts',(-0.861652925570091,-0.144299303100741,
-0.721590372101268));
#12058=CARTESIAN_POINT('Ctrl Pts',(-0.848766861100456,-0.0928409665394229,
-0.736604687327351));
#12059=CARTESIAN_POINT('Ctrl Pts',(-0.84559647055299,-0.0762225747374255,
-0.740223768851063));
#12060=CARTESIAN_POINT('Ctrl Pts',(-0.843383895613249,-0.0595300000000001,
-0.742736168477219));
#12061=CARTESIAN_POINT('',(-0.536443649899847,-0.05953,-0.987512846410683));
#12062=CARTESIAN_POINT('Origin',(0.,-0.05953,0.));
#12063=CARTESIAN_POINT('',(0.0548532617164172,-0.05953,-1.12247250791415));
#12064=CARTESIAN_POINT('Ctrl Pts',(-0.536443649899848,-0.0595300000000001,
-0.987512846410683));
#12065=CARTESIAN_POINT('Ctrl Pts',(-0.533501897135712,-0.0762225747374254,
-0.989110885965947));
#12066=CARTESIAN_POINT('Ctrl Pts',(-0.529268075276156,-0.0928409665394227,
-0.991396466802469));
#12067=CARTESIAN_POINT('Ctrl Pts',(-0.511762781179147,-0.144299303100741,
-1.00061845128527));
#12068=CARTESIAN_POINT('Ctrl Pts',(-0.493462957200432,-0.177024326825049,
-1.0099536580922));
#12069=CARTESIAN_POINT('Ctrl Pts',(-0.45280897844858,-0.227269801620063,
-1.02876878445619));
#12070=CARTESIAN_POINT('Ctrl Pts',(-0.425554672694337,-0.251265615809407,
-1.04048957871266));
#12071=CARTESIAN_POINT('Ctrl Pts',(-0.3787731215897,-0.279889827963178,
-1.05829506364875));
#12072=CARTESIAN_POINT('Ctrl Pts',(-0.354166711873529,-0.290879136862659,
-1.06688848765783));
#12073=CARTESIAN_POINT('Ctrl Pts',(-0.302426893214944,-0.305251990234488,
-1.08269251410343));
#12074=CARTESIAN_POINT('Ctrl Pts',(-0.275287440920027,-0.308638795020976,
-1.0898803575765));
#12075=CARTESIAN_POINT('Ctrl Pts',(-0.224855950742601,-0.308638795020976,
-1.10139101611326));
#12076=CARTESIAN_POINT('Ctrl Pts',(-0.19728546073067,-0.305251990234488,
-1.10669035995599));
#12077=CARTESIAN_POINT('Ctrl Pts',(-0.143812384801039,-0.290879136862659,
-1.11490049012186));
#12078=CARTESIAN_POINT('Ctrl Pts',(-0.117914228755037,-0.279889827963178,
-1.1178344036749));
#12079=CARTESIAN_POINT('Ctrl Pts',(-0.0680399972366989,-0.251265615809407,
-1.12208997038458));
#12080=CARTESIAN_POINT('Ctrl Pts',(-0.0383992541984084,-0.227269801620063,
-1.12335509974011));
#12081=CARTESIAN_POINT('Ctrl Pts',(0.00639229239215326,-0.177024326825049,
-1.12404235695137));
#12082=CARTESIAN_POINT('Ctrl Pts',(0.0269302585198977,-0.144299303100741,
-1.12357162229597));
#12083=CARTESIAN_POINT('Ctrl Pts',(0.04670325263426,-0.0928409665394228,
-1.12285816383385));
#12084=CARTESIAN_POINT('Ctrl Pts',(0.0515094706813703,-0.0762225747374255,
-1.12263591311425));
#12085=CARTESIAN_POINT('Ctrl Pts',(0.0548532617164176,-0.0595300000000001,
-1.12247250791414));
#12086=CARTESIAN_POINT('',(0.437601487681057,-0.05953,-1.03511272300331));
#12087=CARTESIAN_POINT('Origin',(0.,-0.05953,0.));
#12088=CARTESIAN_POINT('',(0.911784794170997,-0.05953,-0.656964154625313));
#12089=CARTESIAN_POINT('Ctrl Pts',(0.437601487681056,-0.0595300000000001,
-1.03511272300331));
#12090=CARTESIAN_POINT('Ctrl Pts',(0.440685038163619,-0.0762225747374255,
-1.03380912944435));
#12091=CARTESIAN_POINT('Ctrl Pts',(0.445111721969657,-0.0928409665394228,
-1.03192403056628));
#12092=CARTESIAN_POINT('Ctrl Pts',(0.463236132117164,-0.144299303100741,
-1.0239876538093));
#12093=CARTESIAN_POINT('Ctrl Pts',(0.481944444320713,-0.177024326825049,
-1.01550068154148));
#12094=CARTESIAN_POINT('Ctrl Pts',(0.522002043615455,-0.227269801620064,
-0.995447160474328));
#12095=CARTESIAN_POINT('Ctrl Pts',(0.548158511259203,-0.251265615809407,
-0.981446681891443));
#12096=CARTESIAN_POINT('Ctrl Pts',(0.591247219971725,-0.279889827963178,
-0.955972930713954));
#12097=CARTESIAN_POINT('Ctrl Pts',(0.613307674922609,-0.290879136862659,
-0.942092777160053));
#12098=CARTESIAN_POINT('Ctrl Pts',(0.657923009631182,-0.305251990234487,
-0.91149460735272));
#12099=CARTESIAN_POINT('Ctrl Pts',(0.680463863683393,-0.308638795020976,
-0.894757676234429));
#12100=CARTESIAN_POINT('Ctrl Pts',(0.720906778729542,-0.308638795020976,
-0.862505527716294));
#12101=CARTESIAN_POINT('Ctrl Pts',(0.742239891936899,-0.305251990234488,
-0.844254137480381));
#12102=CARTESIAN_POINT('Ctrl Pts',(0.781998747691872,-0.290879136862659,
-0.80756613568454));
#12103=CARTESIAN_POINT('Ctrl Pts',(0.800439809856112,-0.279889827963178,
-0.789147407129765));
#12104=CARTESIAN_POINT('Ctrl Pts',(0.834863020612702,-0.251265615809407,
-0.752807465209441));
#12105=CARTESIAN_POINT('Ctrl Pts',(0.854332839576145,-0.227269801620064,
-0.73042219438957));
#12106=CARTESIAN_POINT('Ctrl Pts',(0.882797231409153,-0.177024326825049,
-0.695831250979106));
#12107=CARTESIAN_POINT('Ctrl Pts',(0.895234408667242,-0.144299303100741,
-0.679480524217551));
#12108=CARTESIAN_POINT('Ctrl Pts',(0.907004864562642,-0.0928409665394228,
-0.663576540841106));
#12109=CARTESIAN_POINT('Ctrl Pts',(0.909827729890942,-0.0762225747374256,
-0.659680317203144));
#12110=CARTESIAN_POINT('Ctrl Pts',(0.911784794170998,-0.0595300000000001,
-0.656964154625312));
#12111=CARTESIAN_POINT('',(1.08212377959455,-0.05953,-0.303251606722892));
#12112=CARTESIAN_POINT('Origin',(0.,-0.05953,0.));
#12113=CARTESIAN_POINT('',(1.08212377959455,-0.05953,0.303251606722892));
#12114=CARTESIAN_POINT('Ctrl Pts',(1.08212377959455,-0.0595300000000001,
-0.303251606722892));
#12115=CARTESIAN_POINT('Ctrl Pts',(1.0830271513892,-0.0762225747374255,
-0.300028012588062));
#12116=CARTESIAN_POINT('Ctrl Pts',(1.08431331394788,-0.0928409665394228,
-0.2953917518996));
#12117=CARTESIAN_POINT('Ctrl Pts',(1.08940878963422,-0.144299303100741,
-0.276273267473431));
#12118=CARTESIAN_POINT('Ctrl Pts',(1.09443784939331,-0.177024326825049,
-0.256354979351213));
#12119=CARTESIAN_POINT('Ctrl Pts',(1.10373487993589,-0.227269801620064,
-0.212533521233765));
#12120=CARTESIAN_POINT('Ctrl Pts',(1.10909715583869,-0.251265615809407,
-0.183354415742157));
#12121=CARTESIAN_POINT('Ctrl Pts',(1.1160463456491,-0.279889827963178,-0.133783682657561));
#12122=CARTESIAN_POINT('Ctrl Pts',(1.11894887330541,-0.290879136862659,
-0.107881990270302));
#12123=CARTESIAN_POINT('Ctrl Pts',(1.12284346704144,-0.305251990234488,
-0.0539226701638766));
#12124=CARTESIAN_POINT('Ctrl Pts',(1.123812,-0.308638795020976,-0.025864214957475));
#12125=CARTESIAN_POINT('Ctrl Pts',(1.123812,-0.308638795020976,0.025864214957475));
#12126=CARTESIAN_POINT('Ctrl Pts',(1.12284346704144,-0.305251990234488,
0.0539226701638766));
#12127=CARTESIAN_POINT('Ctrl Pts',(1.11894887330541,-0.290879136862659,
0.107881990270302));
#12128=CARTESIAN_POINT('Ctrl Pts',(1.1160463456491,-0.279889827963178,0.133783682657561));
#12129=CARTESIAN_POINT('Ctrl Pts',(1.10909715583869,-0.251265615809407,
0.183354415742157));
#12130=CARTESIAN_POINT('Ctrl Pts',(1.10373487993589,-0.227269801620064,
0.212533521233765));
#12131=CARTESIAN_POINT('Ctrl Pts',(1.09443784939331,-0.177024326825049,
0.256354979351213));
#12132=CARTESIAN_POINT('Ctrl Pts',(1.08940878963422,-0.144299303100741,
0.276273267473431));
#12133=CARTESIAN_POINT('Ctrl Pts',(1.08431331394788,-0.0928409665394228,
0.2953917518996));
#12134=CARTESIAN_POINT('Ctrl Pts',(1.0830271513892,-0.0762225747374255,
0.300028012588062));
#12135=CARTESIAN_POINT('Ctrl Pts',(1.08212377959455,-0.0595300000000001,
0.303251606722892));
#12136=CARTESIAN_POINT('Origin',(0.,-0.05953,0.));
#12137=CARTESIAN_POINT('Origin',(0.,-0.05953,0.));
#12138=CARTESIAN_POINT('',(0.0589974094846122,-0.05953,1.07456964270265));
#12139=CARTESIAN_POINT('Origin',(0.,-0.05953,0.));
#12140=CARTESIAN_POINT('Origin',(-0.244773027351946,-0.05953,1.07242070340001));
#12141=CARTESIAN_POINT('Origin',(-0.244773027351946,0.,1.07242070340001));
#12142=CARTESIAN_POINT('',(-0.519393123750572,-0.05953,0.942555777842682));
#12143=CARTESIAN_POINT('Ctrl Pts',(-0.519393123750572,-0.05953,0.942555777842682));
#12144=CARTESIAN_POINT('Ctrl Pts',(-0.513714466572041,-0.0925528133349865,
0.945684988399766));
#12145=CARTESIAN_POINT('Ctrl Pts',(-0.503136848051455,-0.124911173756694,
0.951483858396181));
#12146=CARTESIAN_POINT('Ctrl Pts',(-0.47593627990192,-0.177924977804098,
0.965323333309091));
#12147=CARTESIAN_POINT('Ctrl Pts',(-0.460931856495794,-0.199697230012983,
0.972669835243841));
#12148=CARTESIAN_POINT('Ctrl Pts',(-0.426157505475872,-0.237895043532788,
0.988400002689705));
#12149=CARTESIAN_POINT('Ctrl Pts',(-0.406380688682952,-0.254319232363049,
0.996771768218699));
#12150=CARTESIAN_POINT('Ctrl Pts',(-0.364750145543744,-0.28018331644634,
1.01272583306292));
#12151=CARTESIAN_POINT('Ctrl Pts',(-0.340838910881557,-0.29104845371857,
1.02112815447116));
#12152=CARTESIAN_POINT('Ctrl Pts',(-0.290495481564827,-0.30527573347708,
1.036574285215));
#12153=CARTESIAN_POINT('Ctrl Pts',(-0.264056468041074,-0.308638795020976,
1.04359501395068));
#12154=CARTESIAN_POINT('Ctrl Pts',(-0.214892249704082,-0.308638795020976,
1.05481642595959));
#12155=CARTESIAN_POINT('Ctrl Pts',(-0.188025341585962,-0.30527573347708,
1.05996242598502));
#12156=CARTESIAN_POINT('Ctrl Pts',(-0.135965654106109,-0.29104845371857,
1.06788913840721));
#12157=CARTESIAN_POINT('Ctrl Pts',(-0.110776745452494,-0.28018331644634,
1.07069360430242));
#12158=CARTESIAN_POINT('Ctrl Pts',(-0.0663467128214646,-0.254319232363049,
1.07438230428002));
#12159=CARTESIAN_POINT('Ctrl Pts',(-0.0448960436540983,-0.237895043532788,
1.07542044338697));
#12160=CARTESIAN_POINT('Ctrl Pts',(-0.00674037211528124,-0.199697230012983,
1.07633607767727));
#12161=CARTESIAN_POINT('Ctrl Pts',(0.00996567398334777,-0.177924977804098,
1.07622728347683));
#12162=CARTESIAN_POINT('Ctrl Pts',(0.0404772621979741,-0.124911173756694,
1.07556023164702));
#12163=CARTESIAN_POINT('Ctrl Pts',(0.0525234025782719,-0.0925528133349865,
1.07492508698591));
#12164=CARTESIAN_POINT('Ctrl Pts',(0.0589974094846124,-0.05953,1.07456964270265));
#12165=CARTESIAN_POINT('Origin',(-0.244773027351946,-0.05953,1.07242070340001));
#12166=CARTESIAN_POINT('Origin',(0.,-0.05953,0.));
#12167=CARTESIAN_POINT('',(-0.803348093619616,-0.05953,0.716109245731214));
#12168=CARTESIAN_POINT('Origin',(0.,-0.05953,0.));
#12169=CARTESIAN_POINT('Origin',(-0.991065754692661,-0.05953,0.477272113029314));
#12170=CARTESIAN_POINT('Origin',(-0.991065754692661,0.,0.477272113029314));
#12171=CARTESIAN_POINT('',(-1.06075609691358,-0.05953,0.181596019242328));
#12172=CARTESIAN_POINT('Ctrl Pts',(-1.06075609691358,-0.05953,0.181596019242328));
#12173=CARTESIAN_POINT('Ctrl Pts',(-1.05966202740332,-0.0925528133349865,
0.187986803072856));
#12174=CARTESIAN_POINT('Ctrl Pts',(-1.05760072925372,-0.124911173756694,
0.199872254546857));
#12175=CARTESIAN_POINT('Ctrl Pts',(-1.05146158959546,-0.177924977804098,
0.22976728653846));
#12176=CARTESIAN_POINT('Ctrl Pts',(-1.04785021111757,-0.199697230012983,
0.246078686169301));
#12177=CARTESIAN_POINT('Ctrl Pts',(-1.03846709802406,-0.237895043532788,
0.283073967563097));
#12178=CARTESIAN_POINT('Ctrl Pts',(-1.03268176429485,-0.254319232363049,
0.303755815985685));
#12179=CARTESIAN_POINT('Ctrl Pts',(-1.01919893537026,-0.28018331644634,
0.346251081972725));
#12180=CARTESIAN_POINT('Ctrl Pts',(-1.01085972381132,-0.29104845371857,
0.370184399726282));
#12181=CARTESIAN_POINT('Ctrl Pts',(-0.99154738033959,-0.30527573347708,
0.419174982698463));
#12182=CARTESIAN_POINT('Ctrl Pts',(-0.980551951791748,-0.308638795020976,
0.444223188605045));
#12183=CARTESIAN_POINT('Ctrl Pts',(-0.958671816228589,-0.308638795020976,
0.489657758261848));
#12184=CARTESIAN_POINT('Ctrl Pts',(-0.945943877838127,-0.30527573347708,
0.51387163140139));
#12185=CARTESIAN_POINT('Ctrl Pts',(-0.91968254693063,-0.29104845371857,
0.559515758398093));
#12186=CARTESIAN_POINT('Ctrl Pts',(-0.906170138993533,-0.28018331644634,
0.580957796077825));
#12187=CARTESIAN_POINT('Ctrl Pts',(-0.8813524085237,-0.254319232363049,
0.617994461173994));
#12188=CARTESIAN_POINT('Ctrl Pts',(-0.868789784891799,-0.237895043532788,
0.635412538795143));
#12189=CARTESIAN_POINT('Ctrl Pts',(-0.845715984518854,-0.199697230012983,
0.66581473268113));
#12190=CARTESIAN_POINT('Ctrl Pts',(-0.835214876415962,-0.177924977804098,
0.678808213394124));
#12191=CARTESIAN_POINT('Ctrl Pts',(-0.815669690204649,-0.124911173756694,
0.702247233627224));
#12192=CARTESIAN_POINT('Ctrl Pts',(-0.807662468433796,-0.0925528133349865,
0.711269279199861));
#12193=CARTESIAN_POINT('Ctrl Pts',(-0.803348093619616,-0.05953,0.716109245731214));
#12194=CARTESIAN_POINT('Origin',(-0.991065754692661,-0.05953,0.477272113029314));
#12195=CARTESIAN_POINT('Origin',(0.,-0.05953,0.));
#12196=CARTESIAN_POINT('',(-1.076188,-0.05953,1.31795018948079E-16));
#12197=CARTESIAN_POINT('Origin',(0.,-0.05953,0.));
#12198=CARTESIAN_POINT('',(-1.06075609691358,-0.05953,-0.181596019242328));
#12199=CARTESIAN_POINT('Origin',(0.,-0.05953,0.));
#12200=CARTESIAN_POINT('Origin',(-0.991065754692661,-0.05953,-0.477272113029314));
#12201=CARTESIAN_POINT('Origin',(-0.991065754692661,0.,-0.477272113029314));
#12202=CARTESIAN_POINT('',(-0.803348093619616,-0.05953,-0.716109245731215));
#12203=CARTESIAN_POINT('Ctrl Pts',(-0.803348093619616,-0.05953,-0.716109245731215));
#12204=CARTESIAN_POINT('Ctrl Pts',(-0.807662468433795,-0.0925528133349865,
-0.711269279199862));
#12205=CARTESIAN_POINT('Ctrl Pts',(-0.815669690204649,-0.124911173756694,
-0.702247233627224));
#12206=CARTESIAN_POINT('Ctrl Pts',(-0.835214876415962,-0.177924977804098,
-0.678808213394124));
#12207=CARTESIAN_POINT('Ctrl Pts',(-0.845715984518854,-0.199697230012983,
-0.66581473268113));
#12208=CARTESIAN_POINT('Ctrl Pts',(-0.868789784891799,-0.237895043532788,
-0.635412538795143));
#12209=CARTESIAN_POINT('Ctrl Pts',(-0.8813524085237,-0.254319232363049,
-0.617994461173994));
#12210=CARTESIAN_POINT('Ctrl Pts',(-0.906170138993533,-0.28018331644634,
-0.580957796077826));
#12211=CARTESIAN_POINT('Ctrl Pts',(-0.91968254693063,-0.29104845371857,
-0.559515758398093));
#12212=CARTESIAN_POINT('Ctrl Pts',(-0.945943877838127,-0.30527573347708,
-0.51387163140139));
#12213=CARTESIAN_POINT('Ctrl Pts',(-0.958671816228589,-0.308638795020976,
-0.489657758261848));
#12214=CARTESIAN_POINT('Ctrl Pts',(-0.980551951791748,-0.308638795020976,
-0.444223188605045));
#12215=CARTESIAN_POINT('Ctrl Pts',(-0.99154738033959,-0.30527573347708,
-0.419174982698463));
#12216=CARTESIAN_POINT('Ctrl Pts',(-1.01085972381132,-0.29104845371857,
-0.370184399726282));
#12217=CARTESIAN_POINT('Ctrl Pts',(-1.01919893537026,-0.28018331644634,
-0.346251081972725));
#12218=CARTESIAN_POINT('Ctrl Pts',(-1.03268176429485,-0.254319232363049,
-0.303755815985685));
#12219=CARTESIAN_POINT('Ctrl Pts',(-1.03846709802406,-0.237895043532788,
-0.283073967563097));
#12220=CARTESIAN_POINT('Ctrl Pts',(-1.04785021111757,-0.199697230012983,
-0.246078686169302));
#12221=CARTESIAN_POINT('Ctrl Pts',(-1.05146158959546,-0.177924977804098,
-0.229767286538461));
#12222=CARTESIAN_POINT('Ctrl Pts',(-1.05760072925372,-0.124911173756694,
-0.199872254546858));
#12223=CARTESIAN_POINT('Ctrl Pts',(-1.05966202740332,-0.0925528133349864,
-0.187986803072857));
#12224=CARTESIAN_POINT('Ctrl Pts',(-1.06075609691358,-0.05953,-0.181596019242328));
#12225=CARTESIAN_POINT('Origin',(-0.991065754692661,-0.05953,-0.477272113029314));
#12226=CARTESIAN_POINT('Origin',(0.,-0.05953,0.));
#12227=CARTESIAN_POINT('',(-0.519393123750572,-0.05953,-0.942555777842682));
#12228=CARTESIAN_POINT('Origin',(0.,-0.05953,0.));
#12229=CARTESIAN_POINT('Origin',(-0.244773027351946,-0.05953,-1.07242070340001));
#12230=CARTESIAN_POINT('Origin',(-0.244773027351946,0.,-1.07242070340001));
#12231=CARTESIAN_POINT('',(0.0589974094846125,-0.05953,-1.07456964270265));
#12232=CARTESIAN_POINT('Ctrl Pts',(0.0589974094846127,-0.05953,-1.07456964270265));
#12233=CARTESIAN_POINT('Ctrl Pts',(0.0525234025782722,-0.0925528133349865,
-1.07492508698591));
#12234=CARTESIAN_POINT('Ctrl Pts',(0.0404772621979744,-0.124911173756694,
-1.07556023164702));
#12235=CARTESIAN_POINT('Ctrl Pts',(0.0099656739833481,-0.177924977804098,
-1.07622728347683));
#12236=CARTESIAN_POINT('Ctrl Pts',(-0.00674037211528096,-0.199697230012983,
-1.07633607767727));
#12237=CARTESIAN_POINT('Ctrl Pts',(-0.044896043654098,-0.237895043532788,
-1.07542044338697));
#12238=CARTESIAN_POINT('Ctrl Pts',(-0.0663467128214644,-0.254319232363049,
-1.07438230428002));
#12239=CARTESIAN_POINT('Ctrl Pts',(-0.110776745452493,-0.28018331644634,
-1.07069360430242));
#12240=CARTESIAN_POINT('Ctrl Pts',(-0.135965654106109,-0.29104845371857,
-1.06788913840721));
#12241=CARTESIAN_POINT('Ctrl Pts',(-0.188025341585962,-0.30527573347708,
-1.05996242598502));
#12242=CARTESIAN_POINT('Ctrl Pts',(-0.214892249704082,-0.308638795020976,
-1.05481642595959));
#12243=CARTESIAN_POINT('Ctrl Pts',(-0.264056468041074,-0.308638795020976,
-1.04359501395068));
#12244=CARTESIAN_POINT('Ctrl Pts',(-0.290495481564827,-0.30527573347708,
-1.036574285215));
#12245=CARTESIAN_POINT('Ctrl Pts',(-0.340838910881557,-0.291048453718569,
-1.02112815447116));
#12246=CARTESIAN_POINT('Ctrl Pts',(-0.364750145543744,-0.28018331644634,
-1.01272583306292));
#12247=CARTESIAN_POINT('Ctrl Pts',(-0.406380688682952,-0.254319232363049,
-0.996771768218699));
#12248=CARTESIAN_POINT('Ctrl Pts',(-0.426157505475872,-0.237895043532788,
-0.988400002689705));
#12249=CARTESIAN_POINT('Ctrl Pts',(-0.460931856495794,-0.199697230012983,
-0.972669835243841));
#12250=CARTESIAN_POINT('Ctrl Pts',(-0.475936279901919,-0.177924977804098,
-0.965323333309091));
#12251=CARTESIAN_POINT('Ctrl Pts',(-0.503136848051454,-0.124911173756694,
-0.951483858396181));
#12252=CARTESIAN_POINT('Ctrl Pts',(-0.513714466572041,-0.0925528133349865,
-0.945684988399766));
#12253=CARTESIAN_POINT('Ctrl Pts',(-0.519393123750572,-0.05953,-0.942555777842682));
#12254=CARTESIAN_POINT('Origin',(-0.244773027351946,-0.05953,-1.07242070340001));
#12255=CARTESIAN_POINT('Origin',(0.,-0.05953,0.));
#12256=CARTESIAN_POINT('',(0.413083465285518,-0.05953,-0.993751811093549));
#12257=CARTESIAN_POINT('Origin',(0.,-0.05953,0.));
#12258=CARTESIAN_POINT('Origin',(0.685838782044607,-0.05953,-0.860014630714833));
#12259=CARTESIAN_POINT('Origin',(0.685838782044607,0.,-0.860014630714833));
#12260=CARTESIAN_POINT('',(0.876916659919095,-0.05953,-0.623857181492959));
#12261=CARTESIAN_POINT('Ctrl Pts',(0.876916659919095,-0.05953,-0.623857181492958));
#12262=CARTESIAN_POINT('Ctrl Pts',(0.873158080166742,-0.0925528133349865,
-0.62914037979579));
#12263=CARTESIAN_POINT('Ctrl Pts',(0.866144010579847,-0.124911173756694,
-0.638954437806245));
#12264=CARTESIAN_POINT('Ctrl Pts',(0.847641868610495,-0.177924977804098,
-0.663225258065736));
#12265=CARTESIAN_POINT('Ctrl Pts',(0.837310877969633,-0.199697230012983,
-0.676354402927683));
#12266=CARTESIAN_POINT('Ctrl Pts',(0.81280533416753,-0.237895043532788,
-0.705614819529209));
#12267=CARTESIAN_POINT('Ctrl Pts',(0.798619410861634,-0.254319232363049,
-0.721738358858166));
#12268=CARTESIAN_POINT('Ctrl Pts',(0.768033796848072,-0.28018331644634,
-0.754175290318038));
#12269=CARTESIAN_POINT('Ctrl Pts',(0.750136149454208,-0.29104845371857,
-0.772120216227122));
#12270=CARTESIAN_POINT('Ctrl Pts',(0.711480111898423,-0.30527573347708,
-0.807879894508811));
#12271=CARTESIAN_POINT('Ctrl Pts',(0.690705563850638,-0.308638795020976,
-0.825676810575913));
#12272=CARTESIAN_POINT('Ctrl Pts',(0.651278921914856,-0.308638795020976,
-0.857118508332695));
#12273=CARTESIAN_POINT('Ctrl Pts',(0.629305439856167,-0.30527573347708,
-0.873412008702649));
#12274=CARTESIAN_POINT('Ctrl Pts',(0.585840553788742,-0.29104845371857,
-0.903141581680914));
#12275=CARTESIAN_POINT('Ctrl Pts',(0.564362943424239,-0.28018331644634,
-0.916597376014514));
#12276=CARTESIAN_POINT('Ctrl Pts',(0.525933334162556,-0.254319232363049,
-0.939198248544427));
#12277=CARTESIAN_POINT('Ctrl Pts',(0.507057380724533,-0.237895043532788,
-0.949440676105255));
#12278=CARTESIAN_POINT('Ctrl Pts',(0.473077587363686,-0.199697230012983,
-0.966820759530997));
#12279=CARTESIAN_POINT('Ctrl Pts',(0.457978755888596,-0.177924977804098,
-0.973971221090534));
#12280=CARTESIAN_POINT('Ctrl Pts',(0.430199341854858,-0.124911173756694,
-0.986608710139579));
#12281=CARTESIAN_POINT('Ctrl Pts',(0.419070565453384,-0.0925528133349865,
-0.991263089003441));
#12282=CARTESIAN_POINT('Ctrl Pts',(0.413083465285518,-0.05953,-0.993751811093549));
#12283=CARTESIAN_POINT('Origin',(0.685838782044607,-0.05953,-0.860014630714833));
#12284=CARTESIAN_POINT('Origin',(0.,-0.208355,0.));
#12285=CARTESIAN_POINT('',(-1.076188,-0.35718,1.31795018948079E-16));
#12286=CARTESIAN_POINT('Origin',(0.,-0.35718,0.));
#12287=CARTESIAN_POINT('',(-1.076188,-0.208355,1.31795018948079E-16));
#12288=CARTESIAN_POINT('',(1.03449977959455,-0.05953,0.296632461748266));
#12289=CARTESIAN_POINT('Origin',(0.,-0.05953,0.));
#12290=CARTESIAN_POINT('',(1.03449977959455,-0.05953,-0.296632461748266));
#12291=CARTESIAN_POINT('Ctrl Pts',(1.03449977959455,-0.05953,0.296632461748267));
#12292=CARTESIAN_POINT('Ctrl Pts',(1.03628691421076,-0.0925528133349865,
0.290399865505497));
#12293=CARTESIAN_POINT('Ctrl Pts',(1.03958665287714,-0.124911173756694,
0.278797079997872));
#12294=CARTESIAN_POINT('Ctrl Pts',(1.0470264474309,-0.177924977804098,0.249198913998601));
#12295=CARTESIAN_POINT('Ctrl Pts',(1.05084995891418,-0.199697230012983,
0.232935932341942));
#12296=CARTESIAN_POINT('Ctrl Pts',(1.05844771715377,-0.237895043532788,
0.195533155353269));
#12297=CARTESIAN_POINT('Ctrl Pts',(1.06220882929878,-0.254319232363049,
0.17438929156337));
#12298=CARTESIAN_POINT('Ctrl Pts',(1.06849922508772,-0.28018331644634,0.130252399648131));
#12299=CARTESIAN_POINT('Ctrl Pts',(1.07137013248666,-0.29104845371857,0.105070977154072));
#12300=CARTESIAN_POINT('Ctrl Pts',(1.07522652957392,-0.30527573347708,0.0525526752791107));
#12301=CARTESIAN_POINT('Ctrl Pts',(1.076188,-0.308638795020976,0.025214283908933));
#12302=CARTESIAN_POINT('Ctrl Pts',(1.076188,-0.308638795020976,-0.025214283908933));
#12303=CARTESIAN_POINT('Ctrl Pts',(1.07522652957392,-0.30527573347708,-0.0525526752791107));
#12304=CARTESIAN_POINT('Ctrl Pts',(1.07137013248666,-0.29104845371857,-0.105070977154072));
#12305=CARTESIAN_POINT('Ctrl Pts',(1.06849922508772,-0.28018331644634,-0.130252399648131));
#12306=CARTESIAN_POINT('Ctrl Pts',(1.06220882929878,-0.254319232363049,
-0.17438929156337));
#12307=CARTESIAN_POINT('Ctrl Pts',(1.05844771715377,-0.237895043532788,
-0.195533155353269));
#12308=CARTESIAN_POINT('Ctrl Pts',(1.05084995891418,-0.199697230012983,
-0.232935932341942));
#12309=CARTESIAN_POINT('Ctrl Pts',(1.0470264474309,-0.177924977804098,-0.249198913998601));
#12310=CARTESIAN_POINT('Ctrl Pts',(1.03958665287714,-0.124911173756694,
-0.278797079997872));
#12311=CARTESIAN_POINT('Ctrl Pts',(1.03628691421076,-0.0925528133349865,
-0.290399865505497));
#12312=CARTESIAN_POINT('Ctrl Pts',(1.03449977959455,-0.05953,-0.296632461748267));
#12313=CARTESIAN_POINT('Origin',(0.,-0.05953,0.));
#12314=CARTESIAN_POINT('Origin',(0.,-0.05953,0.));
#12315=CARTESIAN_POINT('Origin',(1.1,-0.05953,0.));
#12316=CARTESIAN_POINT('Origin',(1.1,0.,0.));
#12317=CARTESIAN_POINT('Origin',(1.1,-0.05953,0.));
#12318=CARTESIAN_POINT('Origin',(0.,-0.35718,0.));
#12319=CARTESIAN_POINT('Origin',(0.,-0.05953,0.));
#12320=CARTESIAN_POINT('',(0.,0.,0.));
#12321=CARTESIAN_POINT('Origin',(1.119765,0.495,0.));
#12322=CARTESIAN_POINT('',(-1.119765,0.495,-1.37131662304724E-16));
#12323=CARTESIAN_POINT('Origin',(0.,0.495,0.));
#12324=CARTESIAN_POINT('',(-1.085235,0.495,-1.32902956907268E-16));
#12325=CARTESIAN_POINT('Origin',(0.,0.495,0.));
#12326=CARTESIAN_POINT('Origin',(0.,0.4575,0.));
#12327=CARTESIAN_POINT('',(-1.119765,0.42,-1.37131662304724E-16));
#12328=CARTESIAN_POINT('Origin',(0.,0.42,0.));
#12329=CARTESIAN_POINT('',(-1.119765,0.4575,-1.37131662304724E-16));
#12330=CARTESIAN_POINT('Origin',(1.085235,0.42,0.));
#12331=CARTESIAN_POINT('',(-1.085235,0.42,-1.32902956907268E-16));
#12332=CARTESIAN_POINT('Origin',(0.,0.42,0.));
#12333=CARTESIAN_POINT('Origin',(0.,0.4575,0.));
#12334=CARTESIAN_POINT('',(-1.085235,0.4575,-1.32902956907268E-16));
#12335=CARTESIAN_POINT('Origin',(1.119765,-0.42,0.));
#12336=CARTESIAN_POINT('',(-1.119765,-0.42,-1.37131662304724E-16));
#12337=CARTESIAN_POINT('Origin',(0.,-0.42,0.));
#12338=CARTESIAN_POINT('',(-1.085235,-0.42,-1.32902956907268E-16));
#12339=CARTESIAN_POINT('Origin',(0.,-0.42,0.));
#12340=CARTESIAN_POINT('Origin',(0.,-0.4575,0.));
#12341=CARTESIAN_POINT('',(-1.119765,-0.495,-1.37131662304724E-16));
#12342=CARTESIAN_POINT('Origin',(0.,-0.495,0.));
#12343=CARTESIAN_POINT('',(-1.119765,-0.4575,-1.37131662304724E-16));
#12344=CARTESIAN_POINT('Origin',(1.085235,-0.495,0.));
#12345=CARTESIAN_POINT('',(-1.085235,-0.495,-1.32902956907268E-16));
#12346=CARTESIAN_POINT('Origin',(0.,-0.495,0.));
#12347=CARTESIAN_POINT('Origin',(0.,-0.4575,0.));
#12348=CARTESIAN_POINT('',(-1.085235,-0.4575,-1.32902956907268E-16));
#12349=CARTESIAN_POINT('',(0.,0.,0.));
#12350=CARTESIAN_POINT('',(0.,0.,0.));
#12351=CARTESIAN_POINT('',(0.,0.,0.));
#12352=CARTESIAN_POINT('',(0.,0.,0.));
#12353=CARTESIAN_POINT('',(0.,0.,0.));
#12354=CARTESIAN_POINT('',(0.,0.,0.));
#12355=CARTESIAN_POINT('Origin',(0.375,0.5,0.));
#12356=CARTESIAN_POINT('',(-0.375,0.5,-4.59242549680257E-17));
#12357=CARTESIAN_POINT('Origin',(0.,0.5,0.));
#12358=CARTESIAN_POINT('Origin',(0.,0.475,0.));
#12359=CARTESIAN_POINT('',(-0.425,0.45,-5.20474889637625E-17));
#12360=CARTESIAN_POINT('Origin',(0.,0.45,0.));
#12361=CARTESIAN_POINT('',(-0.4,0.475,-4.89858719658941E-17));
#12362=CARTESIAN_POINT('Origin',(0.,0.24,0.));
#12363=CARTESIAN_POINT('',(-0.425,0.0299999999999998,-5.20474889637625E-17));
#12364=CARTESIAN_POINT('Origin',(0.,0.0299999999999998,0.));
#12365=CARTESIAN_POINT('',(-0.425,0.24,-5.20474889637625E-17));
#12366=CARTESIAN_POINT('Origin',(0.,0.0150000000000001,0.));
#12367=CARTESIAN_POINT('',(-0.395,4.85722573273506E-17,-4.83735485663204E-17));
#12368=CARTESIAN_POINT('Origin',(0.,0.,0.));
#12369=CARTESIAN_POINT('',(-0.41,0.0150000000000001,-5.02105187650415E-17));
#12370=CARTESIAN_POINT('Origin',(0.27,0.,0.));
#12371=CARTESIAN_POINT('',(-0.27,0.,-3.30654635769785E-17));
#12372=CARTESIAN_POINT('Origin',(0.,0.,0.));
#12373=CARTESIAN_POINT('Origin',(0.,-0.02,0.));
#12374=CARTESIAN_POINT('',(-0.24505,-0.0498999999999999,3.00099698131059E-17));
#12375=CARTESIAN_POINT('Origin',(0.,-0.0498999999999999,0.));
#12376=CARTESIAN_POINT('',(-0.26,-0.02,-3.18408167778312E-17));
#12377=CARTESIAN_POINT('Origin',(0.,-0.995,0.));
#12378=CARTESIAN_POINT('',(-0.24505,-1.95495,3.00099698131059E-17));
#12379=CARTESIAN_POINT('Origin',(0.,-1.95495,0.));
#12380=CARTESIAN_POINT('',(-0.24505,-0.995,-3.00099698131059E-17));
#12381=CARTESIAN_POINT('Origin',(0.,-1.975,0.));
#12382=CARTESIAN_POINT('',(-0.2,-2.,-2.44929359829471E-17));
#12383=CARTESIAN_POINT('Origin',(0.,-2.,0.));
#12384=CARTESIAN_POINT('',(-0.225,-1.975,-2.75545529808154E-17));
#12385=CARTESIAN_POINT('Origin',(0.,-2.,0.));
#12386=CARTESIAN_POINT('Origin',(0.115470053837925,-0.5,-0.2));
#12387=CARTESIAN_POINT('',(0.23094010767585,-0.5,0.));
#12388=CARTESIAN_POINT('',(0.115470053837925,-0.5,-0.2));
#12389=CARTESIAN_POINT('',(0.23094010767585,-0.5,0.));
#12390=CARTESIAN_POINT('',(0.115470053837925,-0.8,-0.2));
#12391=CARTESIAN_POINT('',(0.115470053837925,-0.5,-0.2));
#12392=CARTESIAN_POINT('',(0.23094010767585,-0.8,0.));
#12393=CARTESIAN_POINT('',(0.23094010767585,-0.8,0.));
#12394=CARTESIAN_POINT('',(0.23094010767585,-0.5,0.));
#12395=CARTESIAN_POINT('Origin',(-0.115470053837925,-0.5,-0.2));
#12396=CARTESIAN_POINT('',(-0.115470053837925,-0.5,-0.2));
#12397=CARTESIAN_POINT('',(0.115470053837925,-0.5,-0.2));
#12398=CARTESIAN_POINT('',(-0.115470053837925,-0.8,-0.2));
#12399=CARTESIAN_POINT('',(-0.115470053837925,-0.5,-0.2));
#12400=CARTESIAN_POINT('',(0.115470053837925,-0.8,-0.2));
#12401=CARTESIAN_POINT('Origin',(-0.23094010767585,-0.5,-2.77555756156289E-17));
#12402=CARTESIAN_POINT('',(-0.23094010767585,-0.5,-2.82820063659975E-17));
#12403=CARTESIAN_POINT('',(-0.115470053837925,-0.5,-0.2));
#12404=CARTESIAN_POINT('',(-0.23094010767585,-0.8,-2.77555756156289E-17));
#12405=CARTESIAN_POINT('',(-0.23094010767585,-0.5,-2.82820063659975E-17));
#12406=CARTESIAN_POINT('',(-0.115470053837925,-0.8,-0.2));
#12407=CARTESIAN_POINT('Origin',(-0.115470053837925,-0.5,0.2));
#12408=CARTESIAN_POINT('',(-0.115470053837925,-0.5,0.2));
#12409=CARTESIAN_POINT('',(-0.23094010767585,-0.5,-2.82820063659975E-17));
#12410=CARTESIAN_POINT('',(-0.115470053837925,-0.8,0.2));
#12411=CARTESIAN_POINT('',(-0.115470053837925,-0.5,0.2));
#12412=CARTESIAN_POINT('',(-0.23094010767585,-0.8,-2.82820063659975E-17));
#12413=CARTESIAN_POINT('Origin',(0.115470053837925,-0.5,0.2));
#12414=CARTESIAN_POINT('',(0.115470053837925,-0.5,0.2));
#12415=CARTESIAN_POINT('',(-0.115470053837925,-0.5,0.2));
#12416=CARTESIAN_POINT('',(0.115470053837925,-0.8,0.2));
#12417=CARTESIAN_POINT('',(0.115470053837925,-0.5,0.2));
#12418=CARTESIAN_POINT('',(-0.115470053837925,-0.8,0.2));
#12419=CARTESIAN_POINT('Origin',(0.23094010767585,-0.5,0.));
#12420=CARTESIAN_POINT('',(0.115470053837925,-0.5,0.2));
#12421=CARTESIAN_POINT('',(0.115470053837925,-0.8,0.2));
#12422=CARTESIAN_POINT('Origin',(0.,-0.5,0.));
#12423=CARTESIAN_POINT('Origin',(0.,-0.8,0.));
#12424=CARTESIAN_POINT('',(0.,0.,0.));
#12425=CARTESIAN_POINT('',(0.,0.,0.));
#12426=CARTESIAN_POINT('Origin',(0.75,1.2,0.));
#12427=CARTESIAN_POINT('',(0.885663593019381,1.2,-0.16));
#12428=CARTESIAN_POINT('',(0.885663593019381,1.2,0.16));
#12429=CARTESIAN_POINT('Origin',(0.,1.2,0.));
#12430=CARTESIAN_POINT('',(0.93,1.2,-0.16));
#12431=CARTESIAN_POINT('',(0.93,1.2,-0.16));
#12432=CARTESIAN_POINT('',(0.93,1.2,0.16));
#12433=CARTESIAN_POINT('',(0.93,1.2,0.16));
#12434=CARTESIAN_POINT('',(0.57,1.2,0.16));
#12435=CARTESIAN_POINT('Origin',(0.57,0.,0.16));
#12436=CARTESIAN_POINT('',(0.885663593019381,-1.2,0.16));
#12437=CARTESIAN_POINT('',(0.885663593019381,0.,0.16));
#12438=CARTESIAN_POINT('',(0.93,-1.2,0.16));
#12439=CARTESIAN_POINT('',(0.93,0.,0.16));
#12440=CARTESIAN_POINT('',(0.57,-1.2,0.16));
#12441=CARTESIAN_POINT('Origin',(0.75,-1.2,0.));
#12442=CARTESIAN_POINT('',(0.885663593019381,-1.2,-0.16));
#12443=CARTESIAN_POINT('Origin',(0.,-1.2,0.));
#12444=CARTESIAN_POINT('',(0.93,-1.2,-0.16));
#12445=CARTESIAN_POINT('',(0.93,-1.2,0.16));
#12446=CARTESIAN_POINT('',(0.93,-1.2,-0.16));
#12447=CARTESIAN_POINT('Origin',(0.93,0.,-0.16));
#12448=CARTESIAN_POINT('',(0.885663593019381,0.,-0.16));
#12449=CARTESIAN_POINT('',(0.93,0.,-0.16));
#12450=CARTESIAN_POINT('Origin',(0.93,0.,0.16));
#12451=CARTESIAN_POINT('Origin',(1.05,1.5,0.));
#12452=CARTESIAN_POINT('',(-1.05,1.5,-1.28587913910472E-16));
#12453=CARTESIAN_POINT('Origin',(0.,1.5,0.));
#12454=CARTESIAN_POINT('',(-0.9,1.5,-1.10218211923262E-16));
#12455=CARTESIAN_POINT('Origin',(0.,1.5,0.));
#12456=CARTESIAN_POINT('Origin',(0.,1.315,0.));
#12457=CARTESIAN_POINT('',(-1.05,1.13,-1.28587913910472E-16));
#12458=CARTESIAN_POINT('Origin',(0.,1.13,0.));
#12459=CARTESIAN_POINT('',(-1.05,1.315,-1.28587913910472E-16));
#12460=CARTESIAN_POINT('Origin',(1.,1.13,0.));
#12461=CARTESIAN_POINT('',(-1.,1.13,-1.22464679914735E-16));
#12462=CARTESIAN_POINT('Origin',(0.,1.13,0.));
#12463=CARTESIAN_POINT('Origin',(0.,1.065,0.));
#12464=CARTESIAN_POINT('',(-1.,1.,-1.22464679914735E-16));
#12465=CARTESIAN_POINT('Origin',(0.,1.,0.));
#12466=CARTESIAN_POINT('',(-1.,1.065,-1.22464679914735E-16));
#12467=CARTESIAN_POINT('Origin',(1.05,1.,0.));
#12468=CARTESIAN_POINT('',(-1.05,1.,-1.28587913910472E-16));
#12469=CARTESIAN_POINT('Origin',(0.,1.,0.));
#12470=CARTESIAN_POINT('Origin',(0.,0.,0.));
#12471=CARTESIAN_POINT('',(-1.05,-1.,-1.28587913910472E-16));
#12472=CARTESIAN_POINT('Origin',(0.,-1.,0.));
#12473=CARTESIAN_POINT('',(-1.05,0.,-1.28587913910472E-16));
#12474=CARTESIAN_POINT('Origin',(1.,-1.,0.));
#12475=CARTESIAN_POINT('',(-1.,-1.,-1.22464679914735E-16));
#12476=CARTESIAN_POINT('Origin',(0.,-1.,0.));
#12477=CARTESIAN_POINT('Origin',(0.,-1.065,0.));
#12478=CARTESIAN_POINT('',(-1.,-1.13,-1.22464679914735E-16));
#12479=CARTESIAN_POINT('Origin',(0.,-1.13,0.));
#12480=CARTESIAN_POINT('',(-1.,-1.065,-1.22464679914735E-16));
#12481=CARTESIAN_POINT('Origin',(1.05,-1.13,0.));
#12482=CARTESIAN_POINT('',(-1.05,-1.13,-1.28587913910472E-16));
#12483=CARTESIAN_POINT('Origin',(0.,-1.13,0.));
#12484=CARTESIAN_POINT('Origin',(0.,-1.315,0.));
#12485=CARTESIAN_POINT('',(-1.05,-1.5,-1.28587913910472E-16));
#12486=CARTESIAN_POINT('Origin',(0.,-1.5,0.));
#12487=CARTESIAN_POINT('',(-1.05,-1.315,-1.28587913910472E-16));
#12488=CARTESIAN_POINT('Origin',(0.9,-1.5,0.));
#12489=CARTESIAN_POINT('',(-0.9,-1.5,-1.10218211923262E-16));
#12490=CARTESIAN_POINT('Origin',(0.,-1.5,0.));
#12491=CARTESIAN_POINT('Origin',(0.,0.,0.));
#12492=CARTESIAN_POINT('',(-0.9,0.,-1.10218211923262E-16));
#12493=CARTESIAN_POINT('',(0.,0.,0.));
#12494=CARTESIAN_POINT('Origin',(0.75,1.2,0.));
#12495=CARTESIAN_POINT('',(0.880582193778639,1.2,0.16));
#12496=CARTESIAN_POINT('',(0.880582193778639,1.2,-0.16));
#12497=CARTESIAN_POINT('Origin',(0.,1.2,0.));
#12498=CARTESIAN_POINT('',(0.583459510163302,1.2,0.16));
#12499=CARTESIAN_POINT('',(0.57,1.2,0.16));
#12500=CARTESIAN_POINT('',(0.583459510163302,1.2,-0.16));
#12501=CARTESIAN_POINT('Origin',(0.,1.2,0.));
#12502=CARTESIAN_POINT('',(0.93,1.2,-0.16));
#12503=CARTESIAN_POINT('Origin',(0.93,0.,-0.16));
#12504=CARTESIAN_POINT('',(0.880582193778639,-1.2,-0.16));
#12505=CARTESIAN_POINT('',(0.880582193778639,0.,-0.16));
#12506=CARTESIAN_POINT('',(0.583459510163302,-1.2,-0.16));
#12507=CARTESIAN_POINT('',(0.583459510163302,0.,-0.16));
#12508=CARTESIAN_POINT('',(0.93,-1.2,-0.16));
#12509=CARTESIAN_POINT('Origin',(0.75,-1.2,0.));
#12510=CARTESIAN_POINT('',(0.880582193778639,-1.2,0.16));
#12511=CARTESIAN_POINT('Origin',(0.,-1.2,0.));
#12512=CARTESIAN_POINT('',(0.583459510163302,-1.2,0.16));
#12513=CARTESIAN_POINT('Origin',(0.,-1.2,0.));
#12514=CARTESIAN_POINT('',(0.57,-1.2,0.16));
#12515=CARTESIAN_POINT('Origin',(0.57,0.,0.16));
#12516=CARTESIAN_POINT('',(0.880582193778639,0.,0.16));
#12517=CARTESIAN_POINT('',(0.583459510163302,0.,0.16));
#12518=CARTESIAN_POINT('Origin',(0.895,1.35,0.));
#12519=CARTESIAN_POINT('',(-0.895,1.35,-1.09605888523688E-16));
#12520=CARTESIAN_POINT('Origin',(0.,1.35,0.));
#12521=CARTESIAN_POINT('',(-0.605,1.35,-7.40911313484149E-17));
#12522=CARTESIAN_POINT('Origin',(0.,1.35,0.));
#12523=CARTESIAN_POINT('Origin',(0.,0.,0.));
#12524=CARTESIAN_POINT('',(-0.895,-1.35,-1.09605888523688E-16));
#12525=CARTESIAN_POINT('Origin',(0.,-1.35,0.));
#12526=CARTESIAN_POINT('',(-0.895,0.,-1.09605888523688E-16));
#12527=CARTESIAN_POINT('Origin',(0.605,-1.35,0.));
#12528=CARTESIAN_POINT('',(-0.605,-1.35,-7.40911313484149E-17));
#12529=CARTESIAN_POINT('Origin',(0.,-1.35,0.));
#12530=CARTESIAN_POINT('Origin',(0.,0.,0.));
#12531=CARTESIAN_POINT('',(-0.605,0.,-7.40911313484149E-17));
#12532=CARTESIAN_POINT('',(0.,0.,0.));
#12533=CARTESIAN_POINT('',(0.,0.,0.));
#12534=CARTESIAN_POINT('',(0.,0.,0.));
#12535=CARTESIAN_POINT('Origin',(0.0866025403784439,-0.4,-0.15));
#12536=CARTESIAN_POINT('',(0.173205080756888,-0.4,0.));
#12537=CARTESIAN_POINT('',(0.0866025403784439,-0.4,-0.15));
#12538=CARTESIAN_POINT('',(0.173205080756888,-0.4,0.));
#12539=CARTESIAN_POINT('',(0.0866025403784439,-0.64,-0.15));
#12540=CARTESIAN_POINT('',(0.0866025403784439,-0.4,-0.15));
#12541=CARTESIAN_POINT('',(0.173205080756888,-0.64,0.));
#12542=CARTESIAN_POINT('',(0.173205080756888,-0.64,0.));
#12543=CARTESIAN_POINT('',(0.173205080756888,-0.4,0.));
#12544=CARTESIAN_POINT('Origin',(-0.0866025403784438,-0.4,-0.15));
#12545=CARTESIAN_POINT('',(-0.0866025403784438,-0.4,-0.15));
#12546=CARTESIAN_POINT('',(0.0866025403784439,-0.4,-0.15));
#12547=CARTESIAN_POINT('',(-0.0866025403784438,-0.64,-0.15));
#12548=CARTESIAN_POINT('',(-0.0866025403784438,-0.4,-0.15));
#12549=CARTESIAN_POINT('',(0.0866025403784439,-0.64,-0.15));
#12550=CARTESIAN_POINT('Origin',(-0.173205080756888,-0.4,-2.77555756156289E-17));
#12551=CARTESIAN_POINT('',(-0.173205080756888,-0.4,-2.12115047744981E-17));
#12552=CARTESIAN_POINT('',(-0.0866025403784438,-0.4,-0.15));
#12553=CARTESIAN_POINT('',(-0.173205080756888,-0.64,-2.77555756156289E-17));
#12554=CARTESIAN_POINT('',(-0.173205080756888,-0.4,-2.12115047744981E-17));
#12555=CARTESIAN_POINT('',(-0.0866025403784438,-0.64,-0.15));
#12556=CARTESIAN_POINT('Origin',(-0.0866025403784439,-0.4,0.15));
#12557=CARTESIAN_POINT('',(-0.0866025403784439,-0.4,0.15));
#12558=CARTESIAN_POINT('',(-0.173205080756888,-0.4,-2.12115047744981E-17));
#12559=CARTESIAN_POINT('',(-0.0866025403784439,-0.64,0.15));
#12560=CARTESIAN_POINT('',(-0.0866025403784439,-0.4,0.15));
#12561=CARTESIAN_POINT('',(-0.173205080756888,-0.64,-2.12115047744981E-17));
#12562=CARTESIAN_POINT('Origin',(0.0866025403784439,-0.4,0.15));
#12563=CARTESIAN_POINT('',(0.0866025403784439,-0.4,0.15));
#12564=CARTESIAN_POINT('',(-0.0866025403784439,-0.4,0.15));
#12565=CARTESIAN_POINT('',(0.0866025403784439,-0.64,0.15));
#12566=CARTESIAN_POINT('',(0.0866025403784439,-0.4,0.15));
#12567=CARTESIAN_POINT('',(-0.0866025403784439,-0.64,0.15));
#12568=CARTESIAN_POINT('Origin',(0.173205080756888,-0.4,0.));
#12569=CARTESIAN_POINT('',(0.0866025403784439,-0.4,0.15));
#12570=CARTESIAN_POINT('',(0.0866025403784439,-0.64,0.15));
#12571=CARTESIAN_POINT('Origin',(0.,-0.4,-2.77555756156289E-17));
#12572=CARTESIAN_POINT('Origin',(0.,-0.64,-2.77555756156289E-17));
#12573=CARTESIAN_POINT('Origin',(0.,-1.,0.));
#12574=CARTESIAN_POINT('',(-0.1954,-1.,2.39295984553393E-17));
#12575=CARTESIAN_POINT('Origin',(0.,-1.,0.));
#12576=CARTESIAN_POINT('Origin',(0.3,0.4,0.));
#12577=CARTESIAN_POINT('',(-0.3,0.4,-3.67394039744206E-17));
#12578=CARTESIAN_POINT('Origin',(0.,0.4,0.));
#12579=CARTESIAN_POINT('Origin',(0.,0.375,0.));
#12580=CARTESIAN_POINT('',(-0.35,0.35,-4.28626379701573E-17));
#12581=CARTESIAN_POINT('Origin',(0.,0.35,0.));
#12582=CARTESIAN_POINT('',(-0.325,0.375,-3.9801020972289E-17));
#12583=CARTESIAN_POINT('Origin',(0.,0.19,0.));
#12584=CARTESIAN_POINT('',(-0.35,0.03,-4.28626379701574E-17));
#12585=CARTESIAN_POINT('Origin',(0.,0.03,0.));
#12586=CARTESIAN_POINT('',(-0.35,0.19,-4.28626379701574E-17));
#12587=CARTESIAN_POINT('Origin',(0.,0.0149999999999999,0.));
#12588=CARTESIAN_POINT('',(-0.32,-3.29597460435593E-17,-3.91886975727153E-17));
#12589=CARTESIAN_POINT('Origin',(0.,0.,0.));
#12590=CARTESIAN_POINT('',(-0.335,0.0149999999999999,-4.10256677714363E-17));
#12591=CARTESIAN_POINT('Origin',(0.22,0.,0.));
#12592=CARTESIAN_POINT('',(-0.22,-6.93889390390723E-18,-2.69422295812418E-17));
#12593=CARTESIAN_POINT('Origin',(0.,0.,0.));
#12594=CARTESIAN_POINT('Origin',(0.,-0.02,0.));
#12595=CARTESIAN_POINT('',(-0.1954,-0.0492,2.39295984553393E-17));
#12596=CARTESIAN_POINT('Origin',(0.,-0.0492,0.));
#12597=CARTESIAN_POINT('',(-0.21,-0.02,-2.57175827820944E-17));
#12598=CARTESIAN_POINT('Origin',(0.,-0.8,0.));
#12599=CARTESIAN_POINT('',(-0.1954,-0.8,-2.39295984553393E-17));
#12600=CARTESIAN_POINT('',(0.,0.,0.));
#12601=CARTESIAN_POINT('',(0.,0.,0.));
#12602=CARTESIAN_POINT('Origin',(0.,5.,4.));
#12603=CARTESIAN_POINT('',(-0.165,5.,4.));
#12604=CARTESIAN_POINT('Origin',(0.,5.,4.));
#12605=CARTESIAN_POINT('',(-0.165,6.5,4.));
#12606=CARTESIAN_POINT('',(-0.165,5.,4.));
#12607=CARTESIAN_POINT('Origin',(0.,6.5,4.));
#12608=CARTESIAN_POINT('Origin',(0.,5.,4.));
#12609=CARTESIAN_POINT('Origin',(0.,-4.6,4.));
#12610=CARTESIAN_POINT('',(-0.165,-4.5,4.));
#12611=CARTESIAN_POINT('Origin',(0.,-4.5,4.));
#12612=CARTESIAN_POINT('',(-0.165,-2.9,4.));
#12613=CARTESIAN_POINT('',(-0.165,-4.6,4.));
#12614=CARTESIAN_POINT('Origin',(0.,-2.9,4.));
#12615=CARTESIAN_POINT('Origin',(0.,-2.9,4.));
#12616=CARTESIAN_POINT('Origin',(-0.2,4.8,3.3));
#12617=CARTESIAN_POINT('',(-0.2,6.2,3.43431457505076));
#12618=CARTESIAN_POINT('',(-0.2,4.8,3.43431457505076));
#12619=CARTESIAN_POINT('',(-0.2,-4.5,3.43431457505076));
#12620=CARTESIAN_POINT('',(-0.2,6.2,3.65));
#12621=CARTESIAN_POINT('',(-0.2,6.2,3.65));
#12622=CARTESIAN_POINT('',(-0.2,4.8,3.65));
#12623=CARTESIAN_POINT('',(-0.2,4.8,3.65));
#12624=CARTESIAN_POINT('',(-0.2,4.8,3.65));
#12625=CARTESIAN_POINT('Origin',(0.,4.8,3.475));
#12626=CARTESIAN_POINT('',(0.2,4.8,3.43431457505076));
#12627=CARTESIAN_POINT('Origin',(0.,4.8,4.));
#12628=CARTESIAN_POINT('',(0.2,4.8,3.65));
#12629=CARTESIAN_POINT('',(0.2,4.8,3.65));
#12630=CARTESIAN_POINT('',(0.2,4.8,3.3));
#12631=CARTESIAN_POINT('Origin',(0.2,4.8,3.65));
#12632=CARTESIAN_POINT('',(0.2,6.2,3.43431457505076));
#12633=CARTESIAN_POINT('',(0.2,-4.5,3.43431457505076));
#12634=CARTESIAN_POINT('',(0.2,6.2,3.65));
#12635=CARTESIAN_POINT('',(0.2,4.8,3.65));
#12636=CARTESIAN_POINT('',(0.2,6.2,3.3));
#12637=CARTESIAN_POINT('Origin',(-0.2,4.8,3.65));
#12638=CARTESIAN_POINT('',(0.2,6.2,3.65));
#12639=CARTESIAN_POINT('Origin',(0.,6.2,3.475));
#12640=CARTESIAN_POINT('Origin',(0.,6.2,4.));
#12641=CARTESIAN_POINT('Origin',(-0.2,-0.7,3.3));
#12642=CARTESIAN_POINT('',(-0.2,0.7,3.43431457505076));
#12643=CARTESIAN_POINT('',(-0.2,-0.7,3.43431457505076));
#12644=CARTESIAN_POINT('',(-0.2,-4.5,3.43431457505076));
#12645=CARTESIAN_POINT('',(-0.2,0.7,3.65));
#12646=CARTESIAN_POINT('',(-0.2,0.7,3.65));
#12647=CARTESIAN_POINT('',(-0.2,-0.7,3.65));
#12648=CARTESIAN_POINT('',(-0.2,-0.7,3.65));
#12649=CARTESIAN_POINT('',(-0.2,-0.7,3.65));
#12650=CARTESIAN_POINT('Origin',(0.,-0.7,3.475));
#12651=CARTESIAN_POINT('',(0.2,-0.7,3.43431457505076));
#12652=CARTESIAN_POINT('Origin',(0.,-0.7,4.));
#12653=CARTESIAN_POINT('',(0.2,-0.7,3.65));
#12654=CARTESIAN_POINT('',(0.2,-0.7,3.65));
#12655=CARTESIAN_POINT('',(0.2,-0.7,3.3));
#12656=CARTESIAN_POINT('Origin',(0.2,-0.7,3.65));
#12657=CARTESIAN_POINT('',(0.2,0.7,3.43431457505076));
#12658=CARTESIAN_POINT('',(0.2,-4.5,3.43431457505076));
#12659=CARTESIAN_POINT('',(0.2,0.7,3.65));
#12660=CARTESIAN_POINT('',(0.2,-0.7,3.65));
#12661=CARTESIAN_POINT('',(0.2,0.7,3.3));
#12662=CARTESIAN_POINT('Origin',(-0.2,-0.7,3.65));
#12663=CARTESIAN_POINT('',(0.2,0.7,3.65));
#12664=CARTESIAN_POINT('Origin',(0.,0.7,3.475));
#12665=CARTESIAN_POINT('Origin',(0.,0.7,4.));
#12666=CARTESIAN_POINT('Origin',(0.,-4.5,4.));
#12667=CARTESIAN_POINT('',(-0.6,6.5,4.));
#12668=CARTESIAN_POINT('Origin',(0.,6.5,4.));
#12669=CARTESIAN_POINT('',(-0.6,-4.5,4.));
#12670=CARTESIAN_POINT('',(-0.6,-4.5,4.));
#12671=CARTESIAN_POINT('Origin',(0.,-4.5,4.));
#12672=CARTESIAN_POINT('Origin',(0.,6.5,4.));
#12673=CARTESIAN_POINT('Origin',(0.,-4.5,4.));
#12674=CARTESIAN_POINT('',(0.,0.,0.));
#12675=CARTESIAN_POINT('Origin',(0.,-2.,4.));
#12676=CARTESIAN_POINT('',(-0.605,-1.,4.));
#12677=CARTESIAN_POINT('Origin',(0.,-1.,4.));
#12678=CARTESIAN_POINT('',(-0.605,-2.,4.));
#12679=CARTESIAN_POINT('',(-0.605,-2.,4.));
#12680=CARTESIAN_POINT('Origin',(0.,-2.,4.));
#12681=CARTESIAN_POINT('Origin',(0.,-2.,4.));
#12682=CARTESIAN_POINT('',(-0.8,-1.,4.));
#12683=CARTESIAN_POINT('Origin',(0.,-1.,4.));
#12684=CARTESIAN_POINT('',(-0.8,-2.,4.));
#12685=CARTESIAN_POINT('',(-0.8,-2.,4.));
#12686=CARTESIAN_POINT('Origin',(0.,-2.,4.));
#12687=CARTESIAN_POINT('Origin',(0.,-1.,4.));
#12688=CARTESIAN_POINT('Origin',(0.,-2.,4.));
#12689=CARTESIAN_POINT('',(0.,0.,0.));
#12690=CARTESIAN_POINT('Origin',(0.,1.,4.));
#12691=CARTESIAN_POINT('',(-0.605,2.,4.));
#12692=CARTESIAN_POINT('Origin',(0.,2.,4.));
#12693=CARTESIAN_POINT('',(-0.605,1.,4.));
#12694=CARTESIAN_POINT('',(-0.605,1.,4.));
#12695=CARTESIAN_POINT('Origin',(0.,1.,4.));
#12696=CARTESIAN_POINT('Origin',(0.,1.,4.));
#12697=CARTESIAN_POINT('',(-0.8,2.,4.));
#12698=CARTESIAN_POINT('Origin',(0.,2.,4.));
#12699=CARTESIAN_POINT('',(-0.8,1.,4.));
#12700=CARTESIAN_POINT('',(-0.8,1.,4.));
#12701=CARTESIAN_POINT('Origin',(0.,1.,4.));
#12702=CARTESIAN_POINT('Origin',(0.,2.,4.));
#12703=CARTESIAN_POINT('Origin',(0.,1.,4.));
#12704=CARTESIAN_POINT('',(0.,0.,0.));
#12705=CARTESIAN_POINT('Origin',(0.,-4.5,4.));
#12706=CARTESIAN_POINT('',(-0.605,-3.,4.));
#12707=CARTESIAN_POINT('Origin',(0.,-3.,4.));
#12708=CARTESIAN_POINT('',(-0.605,-4.5,4.));
#12709=CARTESIAN_POINT('',(-0.605,-4.5,4.));
#12710=CARTESIAN_POINT('Origin',(0.,-4.5,4.));
#12711=CARTESIAN_POINT('Origin',(0.,-4.5,4.));
#12712=CARTESIAN_POINT('',(-0.8,-3.,4.));
#12713=CARTESIAN_POINT('Origin',(0.,-3.,4.));
#12714=CARTESIAN_POINT('',(-0.8,-4.5,4.));
#12715=CARTESIAN_POINT('',(-0.8,-4.5,4.));
#12716=CARTESIAN_POINT('Origin',(0.,-4.5,4.));
#12717=CARTESIAN_POINT('Origin',(0.,-3.,4.));
#12718=CARTESIAN_POINT('Origin',(0.,-4.5,4.));
#12719=CARTESIAN_POINT('',(0.,0.,0.));
#12720=CARTESIAN_POINT('Origin',(0.,3.,4.));
#12721=CARTESIAN_POINT('',(-0.605,4.5,4.));
#12722=CARTESIAN_POINT('Origin',(0.,4.5,4.));
#12723=CARTESIAN_POINT('',(-0.605,3.,4.));
#12724=CARTESIAN_POINT('',(-0.605,3.,4.));
#12725=CARTESIAN_POINT('Origin',(0.,3.,4.));
#12726=CARTESIAN_POINT('Origin',(0.,3.,4.));
#12727=CARTESIAN_POINT('',(-0.8,4.5,4.));
#12728=CARTESIAN_POINT('Origin',(0.,4.5,4.));
#12729=CARTESIAN_POINT('',(-0.8,3.,4.));
#12730=CARTESIAN_POINT('',(-0.8,3.,4.));
#12731=CARTESIAN_POINT('Origin',(0.,3.,4.));
#12732=CARTESIAN_POINT('Origin',(0.,4.5,4.));
#12733=CARTESIAN_POINT('Origin',(0.,3.,4.));
#12734=CARTESIAN_POINT('',(0.,0.,0.));
#12735=CARTESIAN_POINT('Origin',(-0.2,-1.1,3.22));
#12736=CARTESIAN_POINT('',(-0.2,-1.,3.22));
#12737=CARTESIAN_POINT('',(-0.2,-1.,3.43431457505076));
#12738=CARTESIAN_POINT('',(-0.2,-1.,3.61));
#12739=CARTESIAN_POINT('',(-0.2,1.,3.22));
#12740=CARTESIAN_POINT('',(-0.2,-1.1,3.22));
#12741=CARTESIAN_POINT('',(-0.2,1.,3.43431457505076));
#12742=CARTESIAN_POINT('',(-0.2,1.,3.61));
#12743=CARTESIAN_POINT('',(-0.2,-1.1,3.43431457505076));
#12744=CARTESIAN_POINT('Origin',(0.2,-1.1,3.22));
#12745=CARTESIAN_POINT('',(0.2,-1.,3.22));
#12746=CARTESIAN_POINT('',(0.1,-1.,3.22));
#12747=CARTESIAN_POINT('',(0.2,1.,3.22));
#12748=CARTESIAN_POINT('',(0.2,-1.1,3.22));
#12749=CARTESIAN_POINT('',(0.1,1.,3.22));
#12750=CARTESIAN_POINT('Origin',(0.2,-1.1,4.));
#12751=CARTESIAN_POINT('',(0.2,-1.,3.43431457505076));
#12752=CARTESIAN_POINT('',(0.2,-1.,4.));
#12753=CARTESIAN_POINT('',(0.2,1.,3.43431457505076));
#12754=CARTESIAN_POINT('',(0.2,-1.1,3.43431457505076));
#12755=CARTESIAN_POINT('',(0.2,1.,4.));
#12756=CARTESIAN_POINT('Origin',(0.,1.,4.));
#12757=CARTESIAN_POINT('',(-0.9,1.,4.));
#12758=CARTESIAN_POINT('Origin',(0.,1.,4.));
#12759=CARTESIAN_POINT('Origin',(0.,1.,4.));
#12760=CARTESIAN_POINT('Origin',(0.,-1.1,4.));
#12761=CARTESIAN_POINT('Origin',(0.,-1.,4.));
#12762=CARTESIAN_POINT('Origin',(0.,-1.,4.));
#12763=CARTESIAN_POINT('',(-0.9,-0.6,4.));
#12764=CARTESIAN_POINT('Origin',(0.,-0.6,4.));
#12765=CARTESIAN_POINT('',(-0.9,-1.,4.));
#12766=CARTESIAN_POINT('',(-0.9,-1.,4.));
#12767=CARTESIAN_POINT('Origin',(0.,-1.,4.));
#12768=CARTESIAN_POINT('Origin',(0.,-1.,4.));
#12769=CARTESIAN_POINT('',(-0.9,0.6,4.));
#12770=CARTESIAN_POINT('',(-0.9,-1.,4.));
#12771=CARTESIAN_POINT('Origin',(0.,0.6,4.));
#12772=CARTESIAN_POINT('Origin',(0.,-1.,4.));
#12773=CARTESIAN_POINT('Origin',(0.,-0.6,5.));
#12774=CARTESIAN_POINT('',(-2.,0.6,5.));
#12775=CARTESIAN_POINT('Origin',(0.,0.6,5.));
#12776=CARTESIAN_POINT('',(-2.,-0.6,5.));
#12777=CARTESIAN_POINT('',(-2.,-0.6,5.));
#12778=CARTESIAN_POINT('Origin',(0.,-0.6,5.));
#12779=CARTESIAN_POINT('Origin',(0.,0.6,5.));
#12780=CARTESIAN_POINT('Origin',(0.,-0.6,5.));
#12781=CARTESIAN_POINT('',(0.,0.,0.));
#12782=CARTESIAN_POINT('Origin',(2.5,4.9,4.));
#12783=CARTESIAN_POINT('',(2.275,5.,4.));
#12784=CARTESIAN_POINT('Origin',(2.5,5.,4.));
#12785=CARTESIAN_POINT('',(2.275,5.8,4.));
#12786=CARTESIAN_POINT('',(2.275,4.9,4.));
#12787=CARTESIAN_POINT('Origin',(2.5,5.8,4.));
#12788=CARTESIAN_POINT('Origin',(-0.2,4.4,3.22));
#12789=CARTESIAN_POINT('',(-0.2,4.5,3.22));
#12790=CARTESIAN_POINT('',(-0.2,4.5,3.43431457505076));
#12791=CARTESIAN_POINT('',(-0.2,4.5,3.61));
#12792=CARTESIAN_POINT('',(-0.2,6.5,3.22));
#12793=CARTESIAN_POINT('',(-0.2,4.4,3.22));
#12794=CARTESIAN_POINT('',(-0.2,6.5,3.43431457505076));
#12795=CARTESIAN_POINT('',(-0.2,6.5,3.61));
#12796=CARTESIAN_POINT('',(-0.2,4.5,3.43431457505076));
#12797=CARTESIAN_POINT('Origin',(0.2,4.4,3.22));
#12798=CARTESIAN_POINT('',(0.2,4.5,3.22));
#12799=CARTESIAN_POINT('',(0.1,4.5,3.22));
#12800=CARTESIAN_POINT('',(0.2,6.5,3.22));
#12801=CARTESIAN_POINT('',(0.2,4.4,3.22));
#12802=CARTESIAN_POINT('',(0.1,6.5,3.22));
#12803=CARTESIAN_POINT('Origin',(0.2,4.4,4.));
#12804=CARTESIAN_POINT('',(0.2,4.5,3.43431457505076));
#12805=CARTESIAN_POINT('',(0.2,4.5,4.));
#12806=CARTESIAN_POINT('',(0.2,6.5,3.43431457505076));
#12807=CARTESIAN_POINT('',(0.2,4.5,3.43431457505076));
#12808=CARTESIAN_POINT('',(0.2,6.5,4.));
#12809=CARTESIAN_POINT('Origin',(0.,6.5,4.));
#12810=CARTESIAN_POINT('',(-1.2,6.5,4.));
#12811=CARTESIAN_POINT('Origin',(0.,6.5,4.));
#12812=CARTESIAN_POINT('Origin',(0.,6.5,4.));
#12813=CARTESIAN_POINT('Origin',(0.,4.5,4.));
#12814=CARTESIAN_POINT('Origin',(0.,4.5,4.));
#12815=CARTESIAN_POINT('Origin',(2.5,5.,4.));
#12816=CARTESIAN_POINT('',(1.9255437353462,5.8,3.6));
#12817=CARTESIAN_POINT('',(1.9255437353462,5.,3.6));
#12818=CARTESIAN_POINT('',(1.9255437353462,5.,3.6));
#12819=CARTESIAN_POINT('',(1.9255437353462,5.8,4.4));
#12820=CARTESIAN_POINT('Origin',(2.5,5.8,4.));
#12821=CARTESIAN_POINT('',(1.9255437353462,5.,4.4));
#12822=CARTESIAN_POINT('',(1.9255437353462,5.,4.4));
#12823=CARTESIAN_POINT('Origin',(2.5,5.,4.));
#12824=CARTESIAN_POINT('Origin',(1.25,5.,4.));
#12825=CARTESIAN_POINT('',(1.13137084989848,5.,4.4));
#12826=CARTESIAN_POINT('',(2.5,5.,4.4));
#12827=CARTESIAN_POINT('',(1.13137084989848,5.,3.6));
#12828=CARTESIAN_POINT('Origin',(0.,5.,4.));
#12829=CARTESIAN_POINT('',(0.,5.,3.6));
#12830=CARTESIAN_POINT('Origin',(0.,5.,4.4));
#12831=CARTESIAN_POINT('',(1.13137084989848,5.8,4.4));
#12832=CARTESIAN_POINT('',(2.5,5.8,4.4));
#12833=CARTESIAN_POINT('',(1.13137084989848,4.5,4.4));
#12834=CARTESIAN_POINT('Origin',(2.5,5.,3.6));
#12835=CARTESIAN_POINT('',(1.13137084989848,5.8,3.6));
#12836=CARTESIAN_POINT('',(1.13137084989848,4.5,3.6));
#12837=CARTESIAN_POINT('',(0.,5.8,3.6));
#12838=CARTESIAN_POINT('Origin',(1.25,5.8,4.));
#12839=CARTESIAN_POINT('Origin',(0.,5.8,4.));
#12840=CARTESIAN_POINT('Origin',(0.,4.5,4.));
#12841=CARTESIAN_POINT('',(-1.2,4.5,4.));
#12842=CARTESIAN_POINT('',(-1.2,4.5,4.));
#12843=CARTESIAN_POINT('Origin',(0.,4.5,4.));
#12844=CARTESIAN_POINT('Origin',(0.,4.5,4.));
#12845=CARTESIAN_POINT('',(0.,0.,0.));
#12846=CARTESIAN_POINT('Origin',(2.5,5.7,4.));
#12847=CARTESIAN_POINT('',(2.335,5.8,4.));
#12848=CARTESIAN_POINT('Origin',(2.5,5.8,4.));
#12849=CARTESIAN_POINT('',(2.335,6.9,4.));
#12850=CARTESIAN_POINT('',(2.335,5.7,4.));
#12851=CARTESIAN_POINT('Origin',(2.5,6.9,4.));
#12852=CARTESIAN_POINT('Origin',(2.5,6.9,4.));
#12853=CARTESIAN_POINT('Origin',(2.5,5.8,4.));
#12854=CARTESIAN_POINT('',(1.9,8.2,4.));
#12855=CARTESIAN_POINT('Origin',(2.5,8.2,4.));
#12856=CARTESIAN_POINT('',(1.9,5.8,4.));
#12857=CARTESIAN_POINT('',(1.9,5.8,4.));
#12858=CARTESIAN_POINT('Origin',(2.5,5.8,4.));
#12859=CARTESIAN_POINT('Origin',(2.5,8.2,4.));
#12860=CARTESIAN_POINT('Origin',(2.5,5.8,4.));
#12861=CARTESIAN_POINT('',(0.,0.,0.));
#12862=CARTESIAN_POINT('Origin',(0.,-4.7,4.));
#12863=CARTESIAN_POINT('',(-0.225,-4.5,4.));
#12864=CARTESIAN_POINT('Origin',(0.,-4.5,4.));
#12865=CARTESIAN_POINT('',(-0.225,-4.7,4.));
#12866=CARTESIAN_POINT('',(-0.225,-4.7,4.));
#12867=CARTESIAN_POINT('Origin',(0.,-4.7,4.));
#12868=CARTESIAN_POINT('Origin',(0.,-4.7,4.));
#12869=CARTESIAN_POINT('',(-1.,-4.5,4.));
#12870=CARTESIAN_POINT('Origin',(0.,-4.5,4.));
#12871=CARTESIAN_POINT('',(-1.,-4.7,4.));
#12872=CARTESIAN_POINT('',(-1.,-4.7,4.));
#12873=CARTESIAN_POINT('Origin',(0.,-4.7,4.));
#12874=CARTESIAN_POINT('Origin',(0.,-4.5,4.));
#12875=CARTESIAN_POINT('Origin',(0.,-4.7,4.));
#12876=CARTESIAN_POINT('',(0.,0.,0.));
#12877=CARTESIAN_POINT('Origin',(0.,6.5,4.));
#12878=CARTESIAN_POINT('',(-0.225,6.7,4.));
#12879=CARTESIAN_POINT('Origin',(0.,6.7,4.));
#12880=CARTESIAN_POINT('',(-0.225,6.5,4.));
#12881=CARTESIAN_POINT('',(-0.225,6.5,4.));
#12882=CARTESIAN_POINT('Origin',(0.,6.5,4.));
#12883=CARTESIAN_POINT('Origin',(0.,6.5,4.));
#12884=CARTESIAN_POINT('',(-1.,6.7,4.));
#12885=CARTESIAN_POINT('Origin',(0.,6.7,4.));
#12886=CARTESIAN_POINT('',(-1.,6.5,4.));
#12887=CARTESIAN_POINT('',(-1.,6.5,4.));
#12888=CARTESIAN_POINT('Origin',(0.,6.5,4.));
#12889=CARTESIAN_POINT('Origin',(0.,6.7,4.));
#12890=CARTESIAN_POINT('Origin',(0.,6.5,4.));
#12891=CARTESIAN_POINT('',(0.,0.,0.));
#12892=CARTESIAN_POINT('Origin',(0.7,0.,0.25));
#12893=CARTESIAN_POINT('',(0.7,0.16,0.4));
#12894=CARTESIAN_POINT('',(0.7,0.2,0.36));
#12895=CARTESIAN_POINT('',(0.7,0.1675,0.3925));
#12896=CARTESIAN_POINT('',(0.7,-0.16,0.4));
#12897=CARTESIAN_POINT('',(0.7,0.,0.4));
#12898=CARTESIAN_POINT('',(0.7,-0.2,0.36));
#12899=CARTESIAN_POINT('',(0.7,-0.1675,0.3925));
#12900=CARTESIAN_POINT('',(0.7,-0.2,0.04));
#12901=CARTESIAN_POINT('',(0.7,-0.2,0.125));
#12902=CARTESIAN_POINT('',(0.7,-0.16,0.));
#12903=CARTESIAN_POINT('',(0.7,-0.1925,0.0325));
#12904=CARTESIAN_POINT('',(0.7,0.16,0.));
#12905=CARTESIAN_POINT('',(0.7,0.,0.));
#12906=CARTESIAN_POINT('',(0.7,0.2,0.04));
#12907=CARTESIAN_POINT('',(0.7,0.1925,0.0325));
#12908=CARTESIAN_POINT('',(0.7,0.2,0.125));
#12909=CARTESIAN_POINT('Origin',(-0.4,-0.18,0.02));
#12910=CARTESIAN_POINT('',(-0.7,-0.2,0.04));
#12911=CARTESIAN_POINT('',(-0.4,-0.2,0.04));
#12912=CARTESIAN_POINT('',(-0.7,-0.16,0.));
#12913=CARTESIAN_POINT('',(-0.7,-0.1925,0.0325));
#12914=CARTESIAN_POINT('',(-0.4,-0.16,0.));
#12915=CARTESIAN_POINT('Origin',(-0.8,-0.2,0.));
#12916=CARTESIAN_POINT('',(-0.7,-0.2,0.36));
#12917=CARTESIAN_POINT('',(-0.4,-0.2,0.36));
#12918=CARTESIAN_POINT('',(-0.7,-0.2,0.125));
#12919=CARTESIAN_POINT('Origin',(-0.4,-0.18,0.38));
#12920=CARTESIAN_POINT('',(-0.7,-0.16,0.4));
#12921=CARTESIAN_POINT('',(-0.4,-0.16,0.4));
#12922=CARTESIAN_POINT('',(-0.7,-0.1675,0.3925));
#12923=CARTESIAN_POINT('Origin',(0.,0.,0.4));
#12924=CARTESIAN_POINT('',(-0.7,0.16,0.4));
#12925=CARTESIAN_POINT('',(0.4,0.16,0.4));
#12926=CARTESIAN_POINT('',(-0.7,0.,0.4));
#12927=CARTESIAN_POINT('Origin',(-0.7,0.,0.25));
#12928=CARTESIAN_POINT('',(-0.7,0.2,0.36));
#12929=CARTESIAN_POINT('',(-0.7,0.1675,0.3925));
#12930=CARTESIAN_POINT('',(-0.7,0.2,0.04));
#12931=CARTESIAN_POINT('',(-0.7,0.2,0.125));
#12932=CARTESIAN_POINT('',(-0.7,0.16,0.));
#12933=CARTESIAN_POINT('',(-0.7,0.1925,0.0325));
#12934=CARTESIAN_POINT('',(-0.7,0.,0.));
#12935=CARTESIAN_POINT('Origin',(0.4,0.18,0.38));
#12936=CARTESIAN_POINT('',(0.4,0.2,0.36));
#12937=CARTESIAN_POINT('Origin',(0.8,0.2,0.));
#12938=CARTESIAN_POINT('',(0.4,0.2,0.04));
#12939=CARTESIAN_POINT('Origin',(0.4,0.18,0.02));
#12940=CARTESIAN_POINT('',(0.4,0.16,0.));
#12941=CARTESIAN_POINT('Origin',(0.,0.,0.));
#12942=CARTESIAN_POINT('',(0.,0.,0.));
#12943=CARTESIAN_POINT('Origin',(0.3,0.4,0.));
#12944=CARTESIAN_POINT('',(-0.3,0.4,-3.67394039744206E-17));
#12945=CARTESIAN_POINT('Origin',(0.,0.4,0.));
#12946=CARTESIAN_POINT('Origin',(0.,0.375,0.));
#12947=CARTESIAN_POINT('',(-0.35,0.35,-4.28626379701573E-17));
#12948=CARTESIAN_POINT('Origin',(0.,0.35,0.));
#12949=CARTESIAN_POINT('',(-0.325,0.375,-3.9801020972289E-17));
#12950=CARTESIAN_POINT('Origin',(0.,0.19,0.));
#12951=CARTESIAN_POINT('',(-0.35,0.03,-4.28626379701574E-17));
#12952=CARTESIAN_POINT('Origin',(0.,0.03,0.));
#12953=CARTESIAN_POINT('',(-0.35,0.19,-4.28626379701574E-17));
#12954=CARTESIAN_POINT('Origin',(0.,0.0149999999999999,0.));
#12955=CARTESIAN_POINT('',(-0.32,-3.29597460435593E-17,-3.91886975727153E-17));
#12956=CARTESIAN_POINT('Origin',(0.,0.,0.));
#12957=CARTESIAN_POINT('',(-0.335,0.0149999999999999,-4.10256677714363E-17));
#12958=CARTESIAN_POINT('Origin',(0.22,0.,0.));
#12959=CARTESIAN_POINT('',(-0.22,-6.93889390390723E-18,-2.69422295812418E-17));
#12960=CARTESIAN_POINT('Origin',(0.,0.,0.));
#12961=CARTESIAN_POINT('Origin',(0.,-0.02,0.));
#12962=CARTESIAN_POINT('',(-0.1954,-0.0492,2.39295984553393E-17));
#12963=CARTESIAN_POINT('Origin',(0.,-0.0492,0.));
#12964=CARTESIAN_POINT('',(-0.21,-0.02,-2.57175827820944E-17));
#12965=CARTESIAN_POINT('Origin',(0.,-0.8,0.));
#12966=CARTESIAN_POINT('',(-0.1954,-1.5646,2.39295984553393E-17));
#12967=CARTESIAN_POINT('Origin',(0.,-1.5646,0.));
#12968=CARTESIAN_POINT('',(-0.1954,-0.8,-2.39295984553393E-17));
#12969=CARTESIAN_POINT('Origin',(0.,-1.58,0.));
#12970=CARTESIAN_POINT('',(-0.16,-1.6,-1.95943487863577E-17));
#12971=CARTESIAN_POINT('Origin',(0.,-1.6,0.));
#12972=CARTESIAN_POINT('',(-0.18,-1.58,-2.20436423846524E-17));
#12973=CARTESIAN_POINT('Origin',(0.,-1.6,0.));
#12974=CARTESIAN_POINT('Origin',(0.0866025403784439,-0.4,-0.15));
#12975=CARTESIAN_POINT('',(0.173205080756888,-0.4,0.));
#12976=CARTESIAN_POINT('',(0.0866025403784439,-0.4,-0.15));
#12977=CARTESIAN_POINT('',(0.173205080756888,-0.4,0.));
#12978=CARTESIAN_POINT('',(0.0866025403784439,-0.64,-0.15));
#12979=CARTESIAN_POINT('',(0.0866025403784439,-0.4,-0.15));
#12980=CARTESIAN_POINT('',(0.173205080756888,-0.64,0.));
#12981=CARTESIAN_POINT('',(0.173205080756888,-0.64,0.));
#12982=CARTESIAN_POINT('',(0.173205080756888,-0.4,0.));
#12983=CARTESIAN_POINT('Origin',(-0.0866025403784438,-0.4,-0.15));
#12984=CARTESIAN_POINT('',(-0.0866025403784438,-0.4,-0.15));
#12985=CARTESIAN_POINT('',(0.0866025403784439,-0.4,-0.15));
#12986=CARTESIAN_POINT('',(-0.0866025403784438,-0.64,-0.15));
#12987=CARTESIAN_POINT('',(-0.0866025403784438,-0.4,-0.15));
#12988=CARTESIAN_POINT('',(0.0866025403784439,-0.64,-0.15));
#12989=CARTESIAN_POINT('Origin',(-0.173205080756888,-0.4,-2.77555756156289E-17));
#12990=CARTESIAN_POINT('',(-0.173205080756888,-0.4,-2.12115047744981E-17));
#12991=CARTESIAN_POINT('',(-0.0866025403784438,-0.4,-0.15));
#12992=CARTESIAN_POINT('',(-0.173205080756888,-0.64,-2.77555756156289E-17));
#12993=CARTESIAN_POINT('',(-0.173205080756888,-0.4,-2.12115047744981E-17));
#12994=CARTESIAN_POINT('',(-0.0866025403784438,-0.64,-0.15));
#12995=CARTESIAN_POINT('Origin',(-0.0866025403784439,-0.4,0.15));
#12996=CARTESIAN_POINT('',(-0.0866025403784439,-0.4,0.15));
#12997=CARTESIAN_POINT('',(-0.173205080756888,-0.4,-2.12115047744981E-17));
#12998=CARTESIAN_POINT('',(-0.0866025403784439,-0.64,0.15));
#12999=CARTESIAN_POINT('',(-0.0866025403784439,-0.4,0.15));
#13000=CARTESIAN_POINT('',(-0.173205080756888,-0.64,-2.12115047744981E-17));
#13001=CARTESIAN_POINT('Origin',(0.0866025403784439,-0.4,0.15));
#13002=CARTESIAN_POINT('',(0.0866025403784439,-0.4,0.15));
#13003=CARTESIAN_POINT('',(-0.0866025403784439,-0.4,0.15));
#13004=CARTESIAN_POINT('',(0.0866025403784439,-0.64,0.15));
#13005=CARTESIAN_POINT('',(0.0866025403784439,-0.4,0.15));
#13006=CARTESIAN_POINT('',(-0.0866025403784439,-0.64,0.15));
#13007=CARTESIAN_POINT('Origin',(0.173205080756888,-0.4,0.));
#13008=CARTESIAN_POINT('',(0.0866025403784439,-0.4,0.15));
#13009=CARTESIAN_POINT('',(0.0866025403784439,-0.64,0.15));
#13010=CARTESIAN_POINT('Origin',(0.,-0.4,-2.77555756156289E-17));
#13011=CARTESIAN_POINT('Origin',(0.,-0.64,-2.77555756156289E-17));
#13012=CARTESIAN_POINT('',(0.,0.,0.));
#13013=CARTESIAN_POINT('',(0.,0.,0.));
#13014=CARTESIAN_POINT('',(0.,0.,0.));
#13015=CARTESIAN_POINT('',(0.,0.,0.));
#13016=CARTESIAN_POINT('',(0.,0.,0.));
#13017=CARTESIAN_POINT('',(0.,0.,0.));
#13018=CARTESIAN_POINT('',(0.,0.,0.));
#13019=CARTESIAN_POINT('',(0.,0.,0.));
#13020=CARTESIAN_POINT('',(0.,0.,0.));
#13021=CARTESIAN_POINT('',(0.,0.,0.));
#13022=CARTESIAN_POINT('',(0.,0.,0.));
#13023=CARTESIAN_POINT('',(0.,0.,0.));
#13024=CARTESIAN_POINT('',(0.,0.,0.));
#13025=CARTESIAN_POINT('',(-3.,-2.5,1.8));
#13026=CARTESIAN_POINT('',(3.,-2.5,1.8));
#13027=CARTESIAN_POINT('',(0.,-2.5,4.));
#13028=CARTESIAN_POINT('',(1.4142135623731,-3.5,5.41421356237309));
#13029=CARTESIAN_POINT('',(-1.41421356237309,-3.5,5.41421356237309));
#13030=CARTESIAN_POINT('',(-1.4142135623731,-3.5,2.58578643762691));
#13031=CARTESIAN_POINT('',(1.41421356237309,-3.5,2.5857864376269));
#13032=CARTESIAN_POINT('',(1.4142135623731,-1.5,5.41421356237309));
#13033=CARTESIAN_POINT('',(-1.41421356237309,-1.5,5.41421356237309));
#13034=CARTESIAN_POINT('',(-1.4142135623731,-1.5,2.58578643762691));
#13035=CARTESIAN_POINT('',(1.41421356237309,-1.5,2.5857864376269));
#13036=CARTESIAN_POINT('',(-3.,2.5,1.8));
#13037=CARTESIAN_POINT('',(3.,2.5,1.8));
#13038=CARTESIAN_POINT('',(0.,2.5,4.));
#13039=CARTESIAN_POINT('',(1.4142135623731,1.5,5.41421356237309));
#13040=CARTESIAN_POINT('',(-1.4142135623731,1.5,5.41421356237309));
#13041=CARTESIAN_POINT('',(-1.4142135623731,1.5,2.58578643762691));
#13042=CARTESIAN_POINT('',(1.41421356237309,1.5,2.5857864376269));
#13043=CARTESIAN_POINT('',(1.4142135623731,3.5,5.41421356237309));
#13044=CARTESIAN_POINT('',(-1.41421356237309,3.5,5.41421356237309));
#13045=CARTESIAN_POINT('',(-1.4142135623731,3.5,2.58578643762691));
#13046=CARTESIAN_POINT('',(1.41421356237309,3.5,2.5857864376269));
#13047=CARTESIAN_POINT('',(-3.75,0.,2.4));
#13048=CARTESIAN_POINT('',(3.75,0.,2.4));
#13049=CARTESIAN_POINT('',(0.,0.,14.));
#13050=CARTESIAN_POINT('',(0.,0.,18.));
#13051=CARTESIAN_POINT('',(1.06066017177982,1.06066017177982,21.4));
#13052=CARTESIAN_POINT('',(-1.06066017177982,1.06066017177982,21.4));
#13053=CARTESIAN_POINT('',(-1.06066017177982,-1.06066017177982,21.4));
#13054=CARTESIAN_POINT('',(1.06066017177982,-1.06066017177982,21.4));
#13055=CARTESIAN_POINT('',(0.,0.,0.));
#13056=CARTESIAN_POINT('',(0.,0.,0.));
#13057=CARTESIAN_POINT('',(0.,0.,0.));
#13058=CARTESIAN_POINT('',(0.,0.,0.));
#13059=CARTESIAN_POINT('',(0.,0.,0.));
#13060=CARTESIAN_POINT('',(0.,0.,0.));
#13061=CARTESIAN_POINT('',(0.,0.,0.));
#13062=CARTESIAN_POINT('',(0.,0.,0.));
#13063=CARTESIAN_POINT('',(0.,0.,0.));
#13064=CARTESIAN_POINT('',(0.,0.,0.));
#13065=CARTESIAN_POINT('',(0.,0.,3.65));
#13066=CARTESIAN_POINT('',(-4.71342800766205E-31,5.5,3.65));
#13067=CARTESIAN_POINT('',(2.5,5.,4.));
#13068=CARTESIAN_POINT('',(0.,-4.7,4.));
#13069=CARTESIAN_POINT('',(0.,6.7,4.));
#13070=CARTESIAN_POINT('',(0.,0.,0.));
#13071=CARTESIAN_POINT('',(0.,0.,0.));
#13072=CARTESIAN_POINT('Origin',(0.,0.,6.9));
#13073=CARTESIAN_POINT('',(-0.425,-5.20474889637625E-17,7.));
#13074=CARTESIAN_POINT('Origin',(0.,0.,7.));
#13075=CARTESIAN_POINT('',(-0.425,5.20474889637625E-17,7.6));
#13076=CARTESIAN_POINT('',(-0.425,-5.20474889637625E-17,6.9));
#13077=CARTESIAN_POINT('Origin',(0.,0.,7.6));
#13078=CARTESIAN_POINT('Origin',(1.2,0.8,7.));
#13079=CARTESIAN_POINT('',(1.2,0.8,7.));
#13080=CARTESIAN_POINT('',(-1.2,0.8,7.));
#13081=CARTESIAN_POINT('',(1.2,0.8,7.));
#13082=CARTESIAN_POINT('',(-1.2,0.8,7.6));
#13083=CARTESIAN_POINT('',(-1.2,0.8,7.));
#13084=CARTESIAN_POINT('',(1.2,0.8,7.6));
#13085=CARTESIAN_POINT('',(1.2,0.8,7.6));
#13086=CARTESIAN_POINT('',(1.2,0.8,7.));
#13087=CARTESIAN_POINT('Origin',(1.2,-0.8,7.));
#13088=CARTESIAN_POINT('',(1.2,-0.8,7.));
#13089=CARTESIAN_POINT('',(1.2,-0.8,7.));
#13090=CARTESIAN_POINT('',(1.2,-0.8,7.6));
#13091=CARTESIAN_POINT('',(1.2,-0.8,7.6));
#13092=CARTESIAN_POINT('',(1.2,-0.8,7.));
#13093=CARTESIAN_POINT('Origin',(-1.2,-0.8,7.));
#13094=CARTESIAN_POINT('',(-1.2,-0.8,7.));
#13095=CARTESIAN_POINT('',(-1.2,-0.8,7.));
#13096=CARTESIAN_POINT('',(-1.2,-0.8,7.6));
#13097=CARTESIAN_POINT('',(-1.2,-0.8,7.6));
#13098=CARTESIAN_POINT('',(-1.2,-0.8,7.));
#13099=CARTESIAN_POINT('Origin',(-1.2,0.8,7.));
#13100=CARTESIAN_POINT('',(-1.2,0.8,7.));
#13101=CARTESIAN_POINT('',(-1.2,0.8,7.6));
#13102=CARTESIAN_POINT('Origin',(0.,0.,7.6));
#13103=CARTESIAN_POINT('Origin',(0.,0.,7.));
#13104=CARTESIAN_POINT('',(0.,0.,0.));
#13105=CARTESIAN_POINT('Origin',(1.8,-1.8,23.9));
#13106=CARTESIAN_POINT('',(1.525,-1.8,24.));
#13107=CARTESIAN_POINT('Origin',(1.8,-1.8,24.));
#13108=CARTESIAN_POINT('',(1.525,-1.8,25.));
#13109=CARTESIAN_POINT('',(1.525,-1.8,23.9));
#13110=CARTESIAN_POINT('Origin',(1.8,-1.8,25.));
#13111=CARTESIAN_POINT('Origin',(-1.8,1.8,23.9));
#13112=CARTESIAN_POINT('',(-2.075,1.8,24.));
#13113=CARTESIAN_POINT('Origin',(-1.8,1.8,24.));
#13114=CARTESIAN_POINT('',(-2.075,1.8,25.));
#13115=CARTESIAN_POINT('',(-2.075,1.8,23.9));
#13116=CARTESIAN_POINT('Origin',(-1.8,1.8,25.));
#13117=CARTESIAN_POINT('Origin',(-1.8,-1.8,23.9));
#13118=CARTESIAN_POINT('',(-2.075,-1.8,24.));
#13119=CARTESIAN_POINT('Origin',(-1.8,-1.8,24.));
#13120=CARTESIAN_POINT('',(-2.075,-1.8,25.));
#13121=CARTESIAN_POINT('',(-2.075,-1.8,23.9));
#13122=CARTESIAN_POINT('Origin',(-1.8,-1.8,25.));
#13123=CARTESIAN_POINT('Origin',(1.8,1.8,23.9));
#13124=CARTESIAN_POINT('',(1.525,1.8,24.));
#13125=CARTESIAN_POINT('Origin',(1.8,1.8,24.));
#13126=CARTESIAN_POINT('',(1.525,1.8,25.));
#13127=CARTESIAN_POINT('',(1.525,1.8,23.9));
#13128=CARTESIAN_POINT('Origin',(1.8,1.8,25.));
#13129=CARTESIAN_POINT('Origin',(0.,0.,24.));
#13130=CARTESIAN_POINT('',(-2.5,2.5,24.));
#13131=CARTESIAN_POINT('',(-2.5,-2.5,24.));
#13132=CARTESIAN_POINT('',(-2.5,2.5,24.));
#13133=CARTESIAN_POINT('',(2.5,2.5,24.));
#13134=CARTESIAN_POINT('',(2.5,2.5,24.));
#13135=CARTESIAN_POINT('',(2.5,-2.5,24.));
#13136=CARTESIAN_POINT('',(2.5,-2.5,24.));
#13137=CARTESIAN_POINT('',(-2.5,-2.5,24.));
#13138=CARTESIAN_POINT('',(-0.6,-7.34788079488412E-17,24.));
#13139=CARTESIAN_POINT('Origin',(0.,0.,24.));
#13140=CARTESIAN_POINT('Origin',(2.5,2.5,24.));
#13141=CARTESIAN_POINT('',(-2.5,2.5,25.));
#13142=CARTESIAN_POINT('',(-2.5,2.5,24.));
#13143=CARTESIAN_POINT('',(2.5,2.5,25.));
#13144=CARTESIAN_POINT('',(2.5,2.5,25.));
#13145=CARTESIAN_POINT('',(2.5,2.5,24.));
#13146=CARTESIAN_POINT('Origin',(2.5,-2.5,24.));
#13147=CARTESIAN_POINT('',(2.5,-2.5,25.));
#13148=CARTESIAN_POINT('',(2.5,-2.5,25.));
#13149=CARTESIAN_POINT('',(2.5,-2.5,24.));
#13150=CARTESIAN_POINT('Origin',(-2.5,-2.5,24.));
#13151=CARTESIAN_POINT('',(-2.5,-2.5,25.));
#13152=CARTESIAN_POINT('',(-2.5,-2.5,25.));
#13153=CARTESIAN_POINT('',(-2.5,-2.5,24.));
#13154=CARTESIAN_POINT('Origin',(-2.5,2.5,24.));
#13155=CARTESIAN_POINT('',(-2.5,2.5,25.));
#13156=CARTESIAN_POINT('Origin',(0.,0.,25.));
#13157=CARTESIAN_POINT('Origin',(0.,0.,7.));
#13158=CARTESIAN_POINT('',(-0.5,-6.12323399573677E-17,7.6));
#13159=CARTESIAN_POINT('Origin',(0.,0.,7.6));
#13160=CARTESIAN_POINT('',(-0.5,-6.12323399573677E-17,7.));
#13161=CARTESIAN_POINT('',(-0.5,-6.12323399573677E-17,7.));
#13162=CARTESIAN_POINT('Origin',(0.,0.,7.));
#13163=CARTESIAN_POINT('Origin',(0.,0.,7.));
#13164=CARTESIAN_POINT('Origin',(0.,0.,7.6));
#13165=CARTESIAN_POINT('',(-0.6,-7.34788079488412E-17,7.6));
#13166=CARTESIAN_POINT('',(-0.6,-7.34788079488412E-17,7.6));
#13167=CARTESIAN_POINT('Origin',(0.,0.,7.6));
#13168=CARTESIAN_POINT('Origin',(0.,0.,7.6));
#13169=CARTESIAN_POINT('',(0.,0.,0.));
#13170=CARTESIAN_POINT('Origin',(0.,0.,7.6));
#13171=CARTESIAN_POINT('',(-0.605,-7.40911313484149E-17,7.8));
#13172=CARTESIAN_POINT('Origin',(0.,0.,7.8));
#13173=CARTESIAN_POINT('',(-0.605,-7.40911313484149E-17,7.6));
#13174=CARTESIAN_POINT('',(-0.605,-7.40911313484149E-17,7.6));
#13175=CARTESIAN_POINT('Origin',(0.,0.,7.6));
#13176=CARTESIAN_POINT('Origin',(0.,0.,7.6));
#13177=CARTESIAN_POINT('',(-1.25,-1.53080849893419E-16,7.8));
#13178=CARTESIAN_POINT('Origin',(0.,0.,7.8));
#13179=CARTESIAN_POINT('',(-1.25,-1.53080849893419E-16,7.6));
#13180=CARTESIAN_POINT('',(-1.25,-1.53080849893419E-16,7.6));
#13181=CARTESIAN_POINT('Origin',(0.,0.,7.6));
#13182=CARTESIAN_POINT('Origin',(0.,0.,7.8));
#13183=CARTESIAN_POINT('Origin',(0.,0.,7.6));
#13184=CARTESIAN_POINT('',(0.,0.,0.));
#13185=CARTESIAN_POINT('',(0.,0.,0.));
#13186=CARTESIAN_POINT('',(0.,0.,0.));
#13187=CARTESIAN_POINT('',(0.,0.,0.));
#13188=CARTESIAN_POINT('',(0.,0.,0.));
#13189=CARTESIAN_POINT('',(0.,0.,0.));
#13190=UNCERTAINTY_MEASURE_WITH_UNIT(LENGTH_MEASURE(0.001),#13278,
'DISTANCE_ACCURACY_VALUE',
'Maximum model space distance between geometric entities at asserted c
onnectivities');
#13191=UNCERTAINTY_MEASURE_WITH_UNIT(LENGTH_MEASURE(0.001),#13278,
'DISTANCE_ACCURACY_VALUE',
'Maximum model space distance between geometric entities at asserted c
onnectivities');
#13192=UNCERTAINTY_MEASURE_WITH_UNIT(LENGTH_MEASURE(0.001),#13278,
'DISTANCE_ACCURACY_VALUE',
'Maximum model space distance between geometric entities at asserted c
onnectivities');
#13193=UNCERTAINTY_MEASURE_WITH_UNIT(LENGTH_MEASURE(0.001),#13278,
'DISTANCE_ACCURACY_VALUE',
'Maximum model space distance between geometric entities at asserted c
onnectivities');
#13194=UNCERTAINTY_MEASURE_WITH_UNIT(LENGTH_MEASURE(0.001),#13278,
'DISTANCE_ACCURACY_VALUE',
'Maximum model space distance between geometric entities at asserted c
onnectivities');
#13195=UNCERTAINTY_MEASURE_WITH_UNIT(LENGTH_MEASURE(0.001),#13278,
'DISTANCE_ACCURACY_VALUE',
'Maximum model space distance between geometric entities at asserted c
onnectivities');
#13196=UNCERTAINTY_MEASURE_WITH_UNIT(LENGTH_MEASURE(0.001),#13278,
'DISTANCE_ACCURACY_VALUE',
'Maximum model space distance between geometric entities at asserted c
onnectivities');
#13197=UNCERTAINTY_MEASURE_WITH_UNIT(LENGTH_MEASURE(0.001),#13278,
'DISTANCE_ACCURACY_VALUE',
'Maximum model space distance between geometric entities at asserted c
onnectivities');
#13198=UNCERTAINTY_MEASURE_WITH_UNIT(LENGTH_MEASURE(0.001),#13278,
'DISTANCE_ACCURACY_VALUE',
'Maximum model space distance between geometric entities at asserted c
onnectivities');
#13199=UNCERTAINTY_MEASURE_WITH_UNIT(LENGTH_MEASURE(0.001),#13278,
'DISTANCE_ACCURACY_VALUE',
'Maximum model space distance between geometric entities at asserted c
onnectivities');
#13200=UNCERTAINTY_MEASURE_WITH_UNIT(LENGTH_MEASURE(0.001),#13278,
'DISTANCE_ACCURACY_VALUE',
'Maximum model space distance between geometric entities at asserted c
onnectivities');
#13201=UNCERTAINTY_MEASURE_WITH_UNIT(LENGTH_MEASURE(0.001),#13278,
'DISTANCE_ACCURACY_VALUE',
'Maximum model space distance between geometric entities at asserted c
onnectivities');
#13202=UNCERTAINTY_MEASURE_WITH_UNIT(LENGTH_MEASURE(0.001),#13278,
'DISTANCE_ACCURACY_VALUE',
'Maximum model space distance between geometric entities at asserted c
onnectivities');
#13203=UNCERTAINTY_MEASURE_WITH_UNIT(LENGTH_MEASURE(0.001),#13278,
'DISTANCE_ACCURACY_VALUE',
'Maximum model space distance between geometric entities at asserted c
onnectivities');
#13204=UNCERTAINTY_MEASURE_WITH_UNIT(LENGTH_MEASURE(0.001),#13278,
'DISTANCE_ACCURACY_VALUE',
'Maximum model space distance between geometric entities at asserted c
onnectivities');
#13205=UNCERTAINTY_MEASURE_WITH_UNIT(LENGTH_MEASURE(0.001),#13278,
'DISTANCE_ACCURACY_VALUE',
'Maximum model space distance between geometric entities at asserted c
onnectivities');
#13206=UNCERTAINTY_MEASURE_WITH_UNIT(LENGTH_MEASURE(0.001),#13278,
'DISTANCE_ACCURACY_VALUE',
'Maximum model space distance between geometric entities at asserted c
onnectivities');
#13207=UNCERTAINTY_MEASURE_WITH_UNIT(LENGTH_MEASURE(0.001),#13278,
'DISTANCE_ACCURACY_VALUE',
'Maximum model space distance between geometric entities at asserted c
onnectivities');
#13208=UNCERTAINTY_MEASURE_WITH_UNIT(LENGTH_MEASURE(0.001),#13278,
'DISTANCE_ACCURACY_VALUE',
'Maximum model space distance between geometric entities at asserted c
onnectivities');
#13209=UNCERTAINTY_MEASURE_WITH_UNIT(LENGTH_MEASURE(0.001),#13278,
'DISTANCE_ACCURACY_VALUE',
'Maximum model space distance between geometric entities at asserted c
onnectivities');
#13210=UNCERTAINTY_MEASURE_WITH_UNIT(LENGTH_MEASURE(0.001),#13278,
'DISTANCE_ACCURACY_VALUE',
'Maximum model space distance between geometric entities at asserted c
onnectivities');
#13211=UNCERTAINTY_MEASURE_WITH_UNIT(LENGTH_MEASURE(0.001),#13278,
'DISTANCE_ACCURACY_VALUE',
'Maximum model space distance between geometric entities at asserted c
onnectivities');
#13212=UNCERTAINTY_MEASURE_WITH_UNIT(LENGTH_MEASURE(0.001),#13278,
'DISTANCE_ACCURACY_VALUE',
'Maximum model space distance between geometric entities at asserted c
onnectivities');
#13213=UNCERTAINTY_MEASURE_WITH_UNIT(LENGTH_MEASURE(0.001),#13278,
'DISTANCE_ACCURACY_VALUE',
'Maximum model space distance between geometric entities at asserted c
onnectivities');
#13214=UNCERTAINTY_MEASURE_WITH_UNIT(LENGTH_MEASURE(0.001),#13278,
'DISTANCE_ACCURACY_VALUE',
'Maximum model space distance between geometric entities at asserted c
onnectivities');
#13215=UNCERTAINTY_MEASURE_WITH_UNIT(LENGTH_MEASURE(0.001),#13278,
'DISTANCE_ACCURACY_VALUE',
'Maximum model space distance between geometric entities at asserted c
onnectivities');
#13216=UNCERTAINTY_MEASURE_WITH_UNIT(LENGTH_MEASURE(0.001),#13278,
'DISTANCE_ACCURACY_VALUE',
'Maximum model space distance between geometric entities at asserted c
onnectivities');
#13217=UNCERTAINTY_MEASURE_WITH_UNIT(LENGTH_MEASURE(0.001),#13278,
'DISTANCE_ACCURACY_VALUE',
'Maximum model space distance between geometric entities at asserted c
onnectivities');
#13218=UNCERTAINTY_MEASURE_WITH_UNIT(LENGTH_MEASURE(0.001),#13278,
'DISTANCE_ACCURACY_VALUE',
'Maximum model space distance between geometric entities at asserted c
onnectivities');
#13219=UNCERTAINTY_MEASURE_WITH_UNIT(LENGTH_MEASURE(0.001),#13278,
'DISTANCE_ACCURACY_VALUE',
'Maximum model space distance between geometric entities at asserted c
onnectivities');
#13220=UNCERTAINTY_MEASURE_WITH_UNIT(LENGTH_MEASURE(0.001),#13278,
'DISTANCE_ACCURACY_VALUE',
'Maximum model space distance between geometric entities at asserted c
onnectivities');
#13221=UNCERTAINTY_MEASURE_WITH_UNIT(LENGTH_MEASURE(0.001),#13278,
'DISTANCE_ACCURACY_VALUE',
'Maximum model space distance between geometric entities at asserted c
onnectivities');
#13222=UNCERTAINTY_MEASURE_WITH_UNIT(LENGTH_MEASURE(0.001),#13278,
'DISTANCE_ACCURACY_VALUE',
'Maximum model space distance between geometric entities at asserted c
onnectivities');
#13223=UNCERTAINTY_MEASURE_WITH_UNIT(LENGTH_MEASURE(0.001),#13278,
'DISTANCE_ACCURACY_VALUE',
'Maximum model space distance between geometric entities at asserted c
onnectivities');
#13224=UNCERTAINTY_MEASURE_WITH_UNIT(LENGTH_MEASURE(0.001),#13278,
'DISTANCE_ACCURACY_VALUE',
'Maximum model space distance between geometric entities at asserted c
onnectivities');
#13225=UNCERTAINTY_MEASURE_WITH_UNIT(LENGTH_MEASURE(0.001),#13278,
'DISTANCE_ACCURACY_VALUE',
'Maximum model space distance between geometric entities at asserted c
onnectivities');
#13226=UNCERTAINTY_MEASURE_WITH_UNIT(LENGTH_MEASURE(0.001),#13278,
'DISTANCE_ACCURACY_VALUE',
'Maximum model space distance between geometric entities at asserted c
onnectivities');
#13227=UNCERTAINTY_MEASURE_WITH_UNIT(LENGTH_MEASURE(0.001),#13278,
'DISTANCE_ACCURACY_VALUE',
'Maximum model space distance between geometric entities at asserted c
onnectivities');
#13228=UNCERTAINTY_MEASURE_WITH_UNIT(LENGTH_MEASURE(0.001),#13278,
'DISTANCE_ACCURACY_VALUE',
'Maximum model space distance between geometric entities at asserted c
onnectivities');
#13229=UNCERTAINTY_MEASURE_WITH_UNIT(LENGTH_MEASURE(0.001),#13278,
'DISTANCE_ACCURACY_VALUE',
'Maximum model space distance between geometric entities at asserted c
onnectivities');
#13230=UNCERTAINTY_MEASURE_WITH_UNIT(LENGTH_MEASURE(0.001),#13278,
'DISTANCE_ACCURACY_VALUE',
'Maximum model space distance between geometric entities at asserted c
onnectivities');
#13231=UNCERTAINTY_MEASURE_WITH_UNIT(LENGTH_MEASURE(0.001),#13278,
'DISTANCE_ACCURACY_VALUE',
'Maximum model space distance between geometric entities at asserted c
onnectivities');
#13232=UNCERTAINTY_MEASURE_WITH_UNIT(LENGTH_MEASURE(0.001),#13278,
'DISTANCE_ACCURACY_VALUE',
'Maximum model space distance between geometric entities at asserted c
onnectivities');
#13233=UNCERTAINTY_MEASURE_WITH_UNIT(LENGTH_MEASURE(0.001),#13278,
'DISTANCE_ACCURACY_VALUE',
'Maximum model space distance between geometric entities at asserted c
onnectivities');
#13234=(
GEOMETRIC_REPRESENTATION_CONTEXT(3)
GLOBAL_UNCERTAINTY_ASSIGNED_CONTEXT((#13190))
GLOBAL_UNIT_ASSIGNED_CONTEXT((#13278,#13280,#13281))
REPRESENTATION_CONTEXT('','3D')
);
#13235=(
GEOMETRIC_REPRESENTATION_CONTEXT(3)
GLOBAL_UNCERTAINTY_ASSIGNED_CONTEXT((#13191))
GLOBAL_UNIT_ASSIGNED_CONTEXT((#13278,#13280,#13281))
REPRESENTATION_CONTEXT('','3D')
);
#13236=(
GEOMETRIC_REPRESENTATION_CONTEXT(3)
GLOBAL_UNCERTAINTY_ASSIGNED_CONTEXT((#13192))
GLOBAL_UNIT_ASSIGNED_CONTEXT((#13278,#13280,#13281))
REPRESENTATION_CONTEXT('','3D')
);
#13237=(
GEOMETRIC_REPRESENTATION_CONTEXT(3)
GLOBAL_UNCERTAINTY_ASSIGNED_CONTEXT((#13193))
GLOBAL_UNIT_ASSIGNED_CONTEXT((#13278,#13280,#13281))
REPRESENTATION_CONTEXT('','3D')
);
#13238=(
GEOMETRIC_REPRESENTATION_CONTEXT(3)
GLOBAL_UNCERTAINTY_ASSIGNED_CONTEXT((#13194))
GLOBAL_UNIT_ASSIGNED_CONTEXT((#13278,#13280,#13281))
REPRESENTATION_CONTEXT('','3D')
);
#13239=(
GEOMETRIC_REPRESENTATION_CONTEXT(3)
GLOBAL_UNCERTAINTY_ASSIGNED_CONTEXT((#13195))
GLOBAL_UNIT_ASSIGNED_CONTEXT((#13278,#13280,#13281))
REPRESENTATION_CONTEXT('','3D')
);
#13240=(
GEOMETRIC_REPRESENTATION_CONTEXT(3)
GLOBAL_UNCERTAINTY_ASSIGNED_CONTEXT((#13196))
GLOBAL_UNIT_ASSIGNED_CONTEXT((#13278,#13280,#13281))
REPRESENTATION_CONTEXT('','3D')
);
#13241=(
GEOMETRIC_REPRESENTATION_CONTEXT(3)
GLOBAL_UNCERTAINTY_ASSIGNED_CONTEXT((#13197))
GLOBAL_UNIT_ASSIGNED_CONTEXT((#13278,#13280,#13281))
REPRESENTATION_CONTEXT('','3D')
);
#13242=(
GEOMETRIC_REPRESENTATION_CONTEXT(3)
GLOBAL_UNCERTAINTY_ASSIGNED_CONTEXT((#13198))
GLOBAL_UNIT_ASSIGNED_CONTEXT((#13278,#13280,#13281))
REPRESENTATION_CONTEXT('','3D')
);
#13243=(
GEOMETRIC_REPRESENTATION_CONTEXT(3)
GLOBAL_UNCERTAINTY_ASSIGNED_CONTEXT((#13199))
GLOBAL_UNIT_ASSIGNED_CONTEXT((#13278,#13280,#13281))
REPRESENTATION_CONTEXT('','3D')
);
#13244=(
GEOMETRIC_REPRESENTATION_CONTEXT(3)
GLOBAL_UNCERTAINTY_ASSIGNED_CONTEXT((#13200))
GLOBAL_UNIT_ASSIGNED_CONTEXT((#13278,#13280,#13281))
REPRESENTATION_CONTEXT('','3D')
);
#13245=(
GEOMETRIC_REPRESENTATION_CONTEXT(3)
GLOBAL_UNCERTAINTY_ASSIGNED_CONTEXT((#13201))
GLOBAL_UNIT_ASSIGNED_CONTEXT((#13278,#13280,#13281))
REPRESENTATION_CONTEXT('','3D')
);
#13246=(
GEOMETRIC_REPRESENTATION_CONTEXT(3)
GLOBAL_UNCERTAINTY_ASSIGNED_CONTEXT((#13202))
GLOBAL_UNIT_ASSIGNED_CONTEXT((#13278,#13280,#13281))
REPRESENTATION_CONTEXT('','3D')
);
#13247=(
GEOMETRIC_REPRESENTATION_CONTEXT(3)
GLOBAL_UNCERTAINTY_ASSIGNED_CONTEXT((#13203))
GLOBAL_UNIT_ASSIGNED_CONTEXT((#13278,#13280,#13281))
REPRESENTATION_CONTEXT('','3D')
);
#13248=(
GEOMETRIC_REPRESENTATION_CONTEXT(3)
GLOBAL_UNCERTAINTY_ASSIGNED_CONTEXT((#13204))
GLOBAL_UNIT_ASSIGNED_CONTEXT((#13278,#13280,#13281))
REPRESENTATION_CONTEXT('','3D')
);
#13249=(
GEOMETRIC_REPRESENTATION_CONTEXT(3)
GLOBAL_UNCERTAINTY_ASSIGNED_CONTEXT((#13205))
GLOBAL_UNIT_ASSIGNED_CONTEXT((#13278,#13280,#13281))
REPRESENTATION_CONTEXT('','3D')
);
#13250=(
GEOMETRIC_REPRESENTATION_CONTEXT(3)
GLOBAL_UNCERTAINTY_ASSIGNED_CONTEXT((#13206))
GLOBAL_UNIT_ASSIGNED_CONTEXT((#13278,#13280,#13281))
REPRESENTATION_CONTEXT('','3D')
);
#13251=(
GEOMETRIC_REPRESENTATION_CONTEXT(3)
GLOBAL_UNCERTAINTY_ASSIGNED_CONTEXT((#13207))
GLOBAL_UNIT_ASSIGNED_CONTEXT((#13278,#13280,#13281))
REPRESENTATION_CONTEXT('','3D')
);
#13252=(
GEOMETRIC_REPRESENTATION_CONTEXT(3)
GLOBAL_UNCERTAINTY_ASSIGNED_CONTEXT((#13208))
GLOBAL_UNIT_ASSIGNED_CONTEXT((#13278,#13280,#13281))
REPRESENTATION_CONTEXT('','3D')
);
#13253=(
GEOMETRIC_REPRESENTATION_CONTEXT(3)
GLOBAL_UNCERTAINTY_ASSIGNED_CONTEXT((#13209))
GLOBAL_UNIT_ASSIGNED_CONTEXT((#13278,#13280,#13281))
REPRESENTATION_CONTEXT('','3D')
);
#13254=(
GEOMETRIC_REPRESENTATION_CONTEXT(3)
GLOBAL_UNCERTAINTY_ASSIGNED_CONTEXT((#13210))
GLOBAL_UNIT_ASSIGNED_CONTEXT((#13278,#13280,#13281))
REPRESENTATION_CONTEXT('','3D')
);
#13255=(
GEOMETRIC_REPRESENTATION_CONTEXT(3)
GLOBAL_UNCERTAINTY_ASSIGNED_CONTEXT((#13211))
GLOBAL_UNIT_ASSIGNED_CONTEXT((#13278,#13280,#13281))
REPRESENTATION_CONTEXT('','3D')
);
#13256=(
GEOMETRIC_REPRESENTATION_CONTEXT(3)
GLOBAL_UNCERTAINTY_ASSIGNED_CONTEXT((#13212))
GLOBAL_UNIT_ASSIGNED_CONTEXT((#13278,#13280,#13281))
REPRESENTATION_CONTEXT('','3D')
);
#13257=(
GEOMETRIC_REPRESENTATION_CONTEXT(3)
GLOBAL_UNCERTAINTY_ASSIGNED_CONTEXT((#13213))
GLOBAL_UNIT_ASSIGNED_CONTEXT((#13278,#13280,#13281))
REPRESENTATION_CONTEXT('','3D')
);
#13258=(
GEOMETRIC_REPRESENTATION_CONTEXT(3)
GLOBAL_UNCERTAINTY_ASSIGNED_CONTEXT((#13214))
GLOBAL_UNIT_ASSIGNED_CONTEXT((#13278,#13280,#13281))
REPRESENTATION_CONTEXT('','3D')
);
#13259=(
GEOMETRIC_REPRESENTATION_CONTEXT(3)
GLOBAL_UNCERTAINTY_ASSIGNED_CONTEXT((#13215))
GLOBAL_UNIT_ASSIGNED_CONTEXT((#13278,#13280,#13281))
REPRESENTATION_CONTEXT('','3D')
);
#13260=(
GEOMETRIC_REPRESENTATION_CONTEXT(3)
GLOBAL_UNCERTAINTY_ASSIGNED_CONTEXT((#13216))
GLOBAL_UNIT_ASSIGNED_CONTEXT((#13278,#13280,#13281))
REPRESENTATION_CONTEXT('','3D')
);
#13261=(
GEOMETRIC_REPRESENTATION_CONTEXT(3)
GLOBAL_UNCERTAINTY_ASSIGNED_CONTEXT((#13217))
GLOBAL_UNIT_ASSIGNED_CONTEXT((#13278,#13280,#13281))
REPRESENTATION_CONTEXT('','3D')
);
#13262=(
GEOMETRIC_REPRESENTATION_CONTEXT(3)
GLOBAL_UNCERTAINTY_ASSIGNED_CONTEXT((#13218))
GLOBAL_UNIT_ASSIGNED_CONTEXT((#13278,#13280,#13281))
REPRESENTATION_CONTEXT('','3D')
);
#13263=(
GEOMETRIC_REPRESENTATION_CONTEXT(3)
GLOBAL_UNCERTAINTY_ASSIGNED_CONTEXT((#13219))
GLOBAL_UNIT_ASSIGNED_CONTEXT((#13278,#13280,#13281))
REPRESENTATION_CONTEXT('','3D')
);
#13264=(
GEOMETRIC_REPRESENTATION_CONTEXT(3)
GLOBAL_UNCERTAINTY_ASSIGNED_CONTEXT((#13220))
GLOBAL_UNIT_ASSIGNED_CONTEXT((#13278,#13280,#13281))
REPRESENTATION_CONTEXT('','3D')
);
#13265=(
GEOMETRIC_REPRESENTATION_CONTEXT(3)
GLOBAL_UNCERTAINTY_ASSIGNED_CONTEXT((#13221))
GLOBAL_UNIT_ASSIGNED_CONTEXT((#13278,#13280,#13281))
REPRESENTATION_CONTEXT('','3D')
);
#13266=(
GEOMETRIC_REPRESENTATION_CONTEXT(3)
GLOBAL_UNCERTAINTY_ASSIGNED_CONTEXT((#13222))
GLOBAL_UNIT_ASSIGNED_CONTEXT((#13278,#13280,#13281))
REPRESENTATION_CONTEXT('','3D')
);
#13267=(
GEOMETRIC_REPRESENTATION_CONTEXT(3)
GLOBAL_UNCERTAINTY_ASSIGNED_CONTEXT((#13223))
GLOBAL_UNIT_ASSIGNED_CONTEXT((#13278,#13280,#13281))
REPRESENTATION_CONTEXT('','3D')
);
#13268=(
GEOMETRIC_REPRESENTATION_CONTEXT(3)
GLOBAL_UNCERTAINTY_ASSIGNED_CONTEXT((#13224))
GLOBAL_UNIT_ASSIGNED_CONTEXT((#13278,#13280,#13281))
REPRESENTATION_CONTEXT('','3D')
);
#13269=(
GEOMETRIC_REPRESENTATION_CONTEXT(3)
GLOBAL_UNCERTAINTY_ASSIGNED_CONTEXT((#13225))
GLOBAL_UNIT_ASSIGNED_CONTEXT((#13278,#13280,#13281))
REPRESENTATION_CONTEXT('','3D')
);
#13270=(
GEOMETRIC_REPRESENTATION_CONTEXT(3)
GLOBAL_UNCERTAINTY_ASSIGNED_CONTEXT((#13226))
GLOBAL_UNIT_ASSIGNED_CONTEXT((#13278,#13280,#13281))
REPRESENTATION_CONTEXT('','3D')
);
#13271=(
GEOMETRIC_REPRESENTATION_CONTEXT(3)
GLOBAL_UNCERTAINTY_ASSIGNED_CONTEXT((#13227))
GLOBAL_UNIT_ASSIGNED_CONTEXT((#13278,#13280,#13281))
REPRESENTATION_CONTEXT('','3D')
);
#13272=(
GEOMETRIC_REPRESENTATION_CONTEXT(3)
GLOBAL_UNCERTAINTY_ASSIGNED_CONTEXT((#13228))
GLOBAL_UNIT_ASSIGNED_CONTEXT((#13278,#13280,#13281))
REPRESENTATION_CONTEXT('','3D')
);
#13273=(
GEOMETRIC_REPRESENTATION_CONTEXT(3)
GLOBAL_UNCERTAINTY_ASSIGNED_CONTEXT((#13229))
GLOBAL_UNIT_ASSIGNED_CONTEXT((#13278,#13280,#13281))
REPRESENTATION_CONTEXT('','3D')
);
#13274=(
GEOMETRIC_REPRESENTATION_CONTEXT(3)
GLOBAL_UNCERTAINTY_ASSIGNED_CONTEXT((#13230))
GLOBAL_UNIT_ASSIGNED_CONTEXT((#13278,#13280,#13281))
REPRESENTATION_CONTEXT('','3D')
);
#13275=(
GEOMETRIC_REPRESENTATION_CONTEXT(3)
GLOBAL_UNCERTAINTY_ASSIGNED_CONTEXT((#13231))
GLOBAL_UNIT_ASSIGNED_CONTEXT((#13278,#13280,#13281))
REPRESENTATION_CONTEXT('','3D')
);
#13276=(
GEOMETRIC_REPRESENTATION_CONTEXT(3)
GLOBAL_UNCERTAINTY_ASSIGNED_CONTEXT((#13232))
GLOBAL_UNIT_ASSIGNED_CONTEXT((#13278,#13280,#13281))
REPRESENTATION_CONTEXT('','3D')
);
#13277=(
GEOMETRIC_REPRESENTATION_CONTEXT(3)
GLOBAL_UNCERTAINTY_ASSIGNED_CONTEXT((#13233))
GLOBAL_UNIT_ASSIGNED_CONTEXT((#13278,#13280,#13281))
REPRESENTATION_CONTEXT('','3D')
);
#13278=(
LENGTH_UNIT()
NAMED_UNIT(*)
SI_UNIT(.CENTI.,.METRE.)
);
#13279=(
LENGTH_UNIT()
NAMED_UNIT(*)
SI_UNIT($,.METRE.)
);
#13280=(
NAMED_UNIT(*)
PLANE_ANGLE_UNIT()
SI_UNIT($,.RADIAN.)
);
#13281=(
NAMED_UNIT(*)
SI_UNIT($,.STERADIAN.)
SOLID_ANGLE_UNIT()
);
#13282=SHAPE_DEFINITION_REPRESENTATION(#13325,#13439);
#13283=SHAPE_DEFINITION_REPRESENTATION(#13326,#13440);
#13284=SHAPE_DEFINITION_REPRESENTATION(#13327,#13441);
#13285=SHAPE_DEFINITION_REPRESENTATION(#13328,#13442);
#13286=SHAPE_DEFINITION_REPRESENTATION(#13329,#13443);
#13287=SHAPE_DEFINITION_REPRESENTATION(#13330,#13444);
#13288=SHAPE_DEFINITION_REPRESENTATION(#13331,#13445);
#13289=SHAPE_DEFINITION_REPRESENTATION(#13332,#13446);
#13290=SHAPE_DEFINITION_REPRESENTATION(#13333,#13447);
#13291=SHAPE_DEFINITION_REPRESENTATION(#13334,#13448);
#13292=SHAPE_DEFINITION_REPRESENTATION(#13335,#13449);
#13293=SHAPE_DEFINITION_REPRESENTATION(#13336,#13450);
#13294=SHAPE_DEFINITION_REPRESENTATION(#13337,#13451);
#13295=SHAPE_DEFINITION_REPRESENTATION(#13338,#13452);
#13296=SHAPE_DEFINITION_REPRESENTATION(#13339,#13453);
#13297=SHAPE_DEFINITION_REPRESENTATION(#13340,#13454);
#13298=SHAPE_DEFINITION_REPRESENTATION(#13341,#13455);
#13299=SHAPE_DEFINITION_REPRESENTATION(#13342,#13456);
#13300=SHAPE_DEFINITION_REPRESENTATION(#13343,#13457);
#13301=SHAPE_DEFINITION_REPRESENTATION(#13344,#13458);
#13302=SHAPE_DEFINITION_REPRESENTATION(#13345,#13459);
#13303=SHAPE_DEFINITION_REPRESENTATION(#13351,#13460);
#13304=SHAPE_DEFINITION_REPRESENTATION(#13352,#13461);
#13305=SHAPE_DEFINITION_REPRESENTATION(#13353,#13462);
#13306=SHAPE_DEFINITION_REPRESENTATION(#13354,#13463);
#13307=SHAPE_DEFINITION_REPRESENTATION(#13357,#13464);
#13308=SHAPE_DEFINITION_REPRESENTATION(#13358,#13465);
#13309=SHAPE_DEFINITION_REPRESENTATION(#13359,#13466);
#13310=SHAPE_DEFINITION_REPRESENTATION(#13360,#13467);
#13311=SHAPE_DEFINITION_REPRESENTATION(#13361,#13468);
#13312=SHAPE_DEFINITION_REPRESENTATION(#13362,#13469);
#13313=SHAPE_DEFINITION_REPRESENTATION(#13363,#13470);
#13314=SHAPE_DEFINITION_REPRESENTATION(#13364,#13471);
#13315=SHAPE_DEFINITION_REPRESENTATION(#13365,#13472);
#13316=SHAPE_DEFINITION_REPRESENTATION(#13366,#13473);
#13317=SHAPE_DEFINITION_REPRESENTATION(#13367,#13474);
#13318=SHAPE_DEFINITION_REPRESENTATION(#13368,#13475);
#13319=SHAPE_DEFINITION_REPRESENTATION(#13369,#13476);
#13320=SHAPE_DEFINITION_REPRESENTATION(#13370,#13477);
#13321=SHAPE_DEFINITION_REPRESENTATION(#13429,#13478);
#13322=SHAPE_DEFINITION_REPRESENTATION(#13430,#13479);
#13323=SHAPE_DEFINITION_REPRESENTATION(#13431,#13480);
#13324=SHAPE_DEFINITION_REPRESENTATION(#13432,#13481);
#13325=PRODUCT_DEFINITION_SHAPE('',$,#13483);
#13326=PRODUCT_DEFINITION_SHAPE('',$,#13484);
#13327=PRODUCT_DEFINITION_SHAPE('',$,#13485);
#13328=PRODUCT_DEFINITION_SHAPE('',$,#13486);
#13329=PRODUCT_DEFINITION_SHAPE('',$,#13487);
#13330=PRODUCT_DEFINITION_SHAPE('',$,#13488);
#13331=PRODUCT_DEFINITION_SHAPE('',$,#13489);
#13332=PRODUCT_DEFINITION_SHAPE('',$,#13490);
#13333=PRODUCT_DEFINITION_SHAPE('',$,#13491);
#13334=PRODUCT_DEFINITION_SHAPE('',$,#13492);
#13335=PRODUCT_DEFINITION_SHAPE('',$,#13493);
#13336=PRODUCT_DEFINITION_SHAPE('',$,#13494);
#13337=PRODUCT_DEFINITION_SHAPE('',$,#13495);
#13338=PRODUCT_DEFINITION_SHAPE('',$,#13496);
#13339=PRODUCT_DEFINITION_SHAPE('',$,#13497);
#13340=PRODUCT_DEFINITION_SHAPE('',$,#13498);
#13341=PRODUCT_DEFINITION_SHAPE('',$,#13499);
#13342=PRODUCT_DEFINITION_SHAPE('',$,#13500);
#13343=PRODUCT_DEFINITION_SHAPE('',$,#13501);
#13344=PRODUCT_DEFINITION_SHAPE('',$,#13502);
#13345=PRODUCT_DEFINITION_SHAPE('',$,#13503);
#13346=PRODUCT_DEFINITION_SHAPE($,$,#230);
#13347=PRODUCT_DEFINITION_SHAPE($,$,#231);
#13348=PRODUCT_DEFINITION_SHAPE($,$,#232);
#13349=PRODUCT_DEFINITION_SHAPE($,$,#233);
#13350=PRODUCT_DEFINITION_SHAPE($,$,#234);
#13351=PRODUCT_DEFINITION_SHAPE('',$,#13504);
#13352=PRODUCT_DEFINITION_SHAPE('',$,#13505);
#13353=PRODUCT_DEFINITION_SHAPE('',$,#13506);
#13354=PRODUCT_DEFINITION_SHAPE('',$,#13507);
#13355=PRODUCT_DEFINITION_SHAPE($,$,#235);
#13356=PRODUCT_DEFINITION_SHAPE($,$,#236);
#13357=PRODUCT_DEFINITION_SHAPE('',$,#13508);
#13358=PRODUCT_DEFINITION_SHAPE('',$,#13509);
#13359=PRODUCT_DEFINITION_SHAPE('',$,#13510);
#13360=PRODUCT_DEFINITION_SHAPE('',$,#13511);
#13361=PRODUCT_DEFINITION_SHAPE('',$,#13512);
#13362=PRODUCT_DEFINITION_SHAPE('',$,#13513);
#13363=PRODUCT_DEFINITION_SHAPE('',$,#13514);
#13364=PRODUCT_DEFINITION_SHAPE('',$,#13515);
#13365=PRODUCT_DEFINITION_SHAPE('',$,#13516);
#13366=PRODUCT_DEFINITION_SHAPE('',$,#13517);
#13367=PRODUCT_DEFINITION_SHAPE('',$,#13518);
#13368=PRODUCT_DEFINITION_SHAPE('',$,#13519);
#13369=PRODUCT_DEFINITION_SHAPE('',$,#13520);
#13370=PRODUCT_DEFINITION_SHAPE('',$,#13521);
#13371=PRODUCT_DEFINITION_SHAPE($,$,#237);
#13372=PRODUCT_DEFINITION_SHAPE($,$,#238);
#13373=PRODUCT_DEFINITION_SHAPE($,$,#239);
#13374=PRODUCT_DEFINITION_SHAPE($,$,#240);
#13375=PRODUCT_DEFINITION_SHAPE($,$,#241);
#13376=PRODUCT_DEFINITION_SHAPE($,$,#242);
#13377=PRODUCT_DEFINITION_SHAPE($,$,#243);
#13378=PRODUCT_DEFINITION_SHAPE($,$,#244);
#13379=PRODUCT_DEFINITION_SHAPE($,$,#245);
#13380=PRODUCT_DEFINITION_SHAPE($,$,#246);
#13381=PRODUCT_DEFINITION_SHAPE($,$,#247);
#13382=PRODUCT_DEFINITION_SHAPE($,$,#248);
#13383=PRODUCT_DEFINITION_SHAPE($,$,#249);
#13384=PRODUCT_DEFINITION_SHAPE($,$,#250);
#13385=PRODUCT_DEFINITION_SHAPE($,$,#251);
#13386=PRODUCT_DEFINITION_SHAPE($,$,#252);
#13387=PRODUCT_DEFINITION_SHAPE($,$,#253);
#13388=PRODUCT_DEFINITION_SHAPE($,$,#254);
#13389=PRODUCT_DEFINITION_SHAPE($,$,#255);
#13390=PRODUCT_DEFINITION_SHAPE($,$,#256);
#13391=PRODUCT_DEFINITION_SHAPE($,$,#257);
#13392=PRODUCT_DEFINITION_SHAPE($,$,#258);
#13393=PRODUCT_DEFINITION_SHAPE($,$,#259);
#13394=PRODUCT_DEFINITION_SHAPE($,$,#260);
#13395=PRODUCT_DEFINITION_SHAPE($,$,#261);
#13396=PRODUCT_DEFINITION_SHAPE($,$,#262);
#13397=PRODUCT_DEFINITION_SHAPE($,$,#263);
#13398=PRODUCT_DEFINITION_SHAPE($,$,#264);
#13399=PRODUCT_DEFINITION_SHAPE($,$,#265);
#13400=PRODUCT_DEFINITION_SHAPE($,$,#266);
#13401=PRODUCT_DEFINITION_SHAPE($,$,#267);
#13402=PRODUCT_DEFINITION_SHAPE($,$,#268);
#13403=PRODUCT_DEFINITION_SHAPE($,$,#269);
#13404=PRODUCT_DEFINITION_SHAPE($,$,#270);
#13405=PRODUCT_DEFINITION_SHAPE($,$,#271);
#13406=PRODUCT_DEFINITION_SHAPE($,$,#272);
#13407=PRODUCT_DEFINITION_SHAPE($,$,#273);
#13408=PRODUCT_DEFINITION_SHAPE($,$,#274);
#13409=PRODUCT_DEFINITION_SHAPE($,$,#275);
#13410=PRODUCT_DEFINITION_SHAPE($,$,#276);
#13411=PRODUCT_DEFINITION_SHAPE($,$,#277);
#13412=PRODUCT_DEFINITION_SHAPE($,$,#278);
#13413=PRODUCT_DEFINITION_SHAPE($,$,#279);
#13414=PRODUCT_DEFINITION_SHAPE($,$,#280);
#13415=PRODUCT_DEFINITION_SHAPE($,$,#281);
#13416=PRODUCT_DEFINITION_SHAPE($,$,#282);
#13417=PRODUCT_DEFINITION_SHAPE($,$,#283);
#13418=PRODUCT_DEFINITION_SHAPE($,$,#284);
#13419=PRODUCT_DEFINITION_SHAPE($,$,#285);
#13420=PRODUCT_DEFINITION_SHAPE($,$,#286);
#13421=PRODUCT_DEFINITION_SHAPE($,$,#287);
#13422=PRODUCT_DEFINITION_SHAPE($,$,#288);
#13423=PRODUCT_DEFINITION_SHAPE($,$,#289);
#13424=PRODUCT_DEFINITION_SHAPE($,$,#290);
#13425=PRODUCT_DEFINITION_SHAPE($,$,#291);
#13426=PRODUCT_DEFINITION_SHAPE($,$,#292);
#13427=PRODUCT_DEFINITION_SHAPE($,$,#293);
#13428=PRODUCT_DEFINITION_SHAPE($,$,#294);
#13429=PRODUCT_DEFINITION_SHAPE('',$,#13522);
#13430=PRODUCT_DEFINITION_SHAPE('',$,#13523);
#13431=PRODUCT_DEFINITION_SHAPE('',$,#13524);
#13432=PRODUCT_DEFINITION_SHAPE('',$,#13525);
#13433=PRODUCT_DEFINITION_SHAPE($,$,#295);
#13434=PRODUCT_DEFINITION_SHAPE($,$,#296);
#13435=PRODUCT_DEFINITION_SHAPE($,$,#297);
#13436=PRODUCT_DEFINITION_SHAPE($,$,#298);
#13437=PRODUCT_DEFINITION_SHAPE($,$,#299);
#13438=PRODUCT_DEFINITION_SHAPE($,$,#300);
#13439=SHAPE_REPRESENTATION('',(#6853,#7666,#7667,#7668),#13234);
#13440=SHAPE_REPRESENTATION('',(#6854,#7558,#7559,#7560,#7561,#7562,#7563,
#7564,#7565,#7566,#7567,#7568,#7569,#7570,#7571,#7572,#7573,#7574,#7575,
#7576,#7577,#7578,#7579,#7580,#7581,#7582,#7583,#7584,#7585,#7586,#7587,
#7588,#7589,#7590,#7591,#7592,#7593,#7594,#7595,#7596,#7597,#7598,#7599,
#7600),#13235);
#13441=SHAPE_REPRESENTATION('',(#6855),#13236);
#13442=SHAPE_REPRESENTATION('',(#6885),#13237);
#13443=SHAPE_REPRESENTATION('',(#6892),#13238);
#13444=SHAPE_REPRESENTATION('',(#6899),#13239);
#13445=SHAPE_REPRESENTATION('',(#6931),#13240);
#13446=SHAPE_REPRESENTATION('',(#6956),#13241);
#13447=SHAPE_REPRESENTATION('',(#6981),#13242);
#13448=SHAPE_REPRESENTATION('',(#7013),#13243);
#13449=SHAPE_REPRESENTATION('',(#7038),#13244);
#13450=SHAPE_REPRESENTATION('',(#7063),#13245);
#13451=SHAPE_REPRESENTATION('',(#7115),#13246);
#13452=SHAPE_REPRESENTATION('',(#7124),#13247);
#13453=SHAPE_REPRESENTATION('',(#7149),#13248);
#13454=SHAPE_REPRESENTATION('',(#7154,#7277,#7278,#7279,#7280,#7281),#13249);
#13455=SHAPE_REPRESENTATION('',(#7155),#13250);
#13456=SHAPE_REPRESENTATION('',(#7175),#13251);
#13457=SHAPE_REPRESENTATION('',(#7195),#13252);
#13458=SHAPE_REPRESENTATION('',(#7210),#13253);
#13459=SHAPE_REPRESENTATION('',(#7260),#13254);
#13460=SHAPE_REPRESENTATION('',(#7282),#13255);
#13461=SHAPE_REPRESENTATION('',(#7308,#7358,#7359),#13256);
#13462=SHAPE_REPRESENTATION('',(#7309),#13257);
#13463=SHAPE_REPRESENTATION('',(#7341),#13258);
#13464=SHAPE_REPRESENTATION('',(#7360),#13259);
#13465=SHAPE_REPRESENTATION('',(#7384,#7601,#7602,#7603,#7604,#7605,#7606,
#7607,#7608,#7609,#7610,#7611,#7612,#7613,#7614,#7615),#13260);
#13466=SHAPE_REPRESENTATION('',(#7385),#13261);
#13467=SHAPE_REPRESENTATION('',(#7413),#13262);
#13468=SHAPE_REPRESENTATION('',(#7422),#13263);
#13469=SHAPE_REPRESENTATION('',(#7431),#13264);
#13470=SHAPE_REPRESENTATION('',(#7440),#13265);
#13471=SHAPE_REPRESENTATION('',(#7449),#13266);
#13472=SHAPE_REPRESENTATION('',(#7469),#13267);
#13473=SHAPE_REPRESENTATION('',(#7493),#13268);
#13474=SHAPE_REPRESENTATION('',(#7503),#13269);
#13475=SHAPE_REPRESENTATION('',(#7512),#13270);
#13476=SHAPE_REPRESENTATION('',(#7521),#13271);
#13477=SHAPE_REPRESENTATION('',(#7532),#13272);
#13478=SHAPE_REPRESENTATION('',(#7616,#7663,#7664,#7665),#13273);
#13479=SHAPE_REPRESENTATION('',(#7617),#13274);
#13480=SHAPE_REPRESENTATION('',(#7627),#13275);
#13481=SHAPE_REPRESENTATION('',(#7654),#13276);
#13482=PRODUCT_DEFINITION_CONTEXT('part definition',#13613,'design');
#13483=PRODUCT_DEFINITION('PAT-018','PAT-018',#13526,
#13482);
#13484=PRODUCT_DEFINITION('Bearing frame and stem guide',
'Bearing frame and stem guide',#13527,#13482);
#13485=PRODUCT_DEFINITION('Base','Base',#13528,#13482);
#13486=PRODUCT_DEFINITION('Foot','Foot',#13529,#13482);
#13487=PRODUCT_DEFINITION('Foot (1)','Foot (1)',#13530,#13482);
#13488=PRODUCT_DEFINITION('Camshaft bearing post',
'Camshaft bearing post',#13531,#13482);
#13489=PRODUCT_DEFINITION('Bearing cap','Bearing cap',#13532,#13482);
#13490=PRODUCT_DEFINITION('Bearing cap (1)','Bearing cap (1)',#13533,#13482);
#13491=PRODUCT_DEFINITION('Camshaft bearing post (1)',
'Camshaft bearing post (1)',#13534,#13482);
#13492=PRODUCT_DEFINITION('Bearing cap (2)','Bearing cap (2)',#13535,#13482);
#13493=PRODUCT_DEFINITION('Bearing cap (3)','Bearing cap (3)',#13536,#13482);
#13494=PRODUCT_DEFINITION('Slide guide bridge','Slide guide bridge',#13537,
#13482);
#13495=PRODUCT_DEFINITION('Bushing separator','Bushing separator',#13538,
#13482);
#13496=PRODUCT_DEFINITION('Stem guide cap','Stem guide cap',#13539,#13482);
#13497=PRODUCT_DEFINITION('Installed return spring',
'Installed return spring',#13540,#13482);
#13498=PRODUCT_DEFINITION('Sealed Ball Bearing - 12 x 32 x 10 mm',
'Sealed Ball Bearing - 12 x 32 x 10 mm',#13541,#13482);
#13499=PRODUCT_DEFINITION('Inner ring','Inner ring',#13542,#13482);
#13500=PRODUCT_DEFINITION('Outer ring','Outer ring',#13543,#13482);
#13501=PRODUCT_DEFINITION('Balls','Balls',#13544,#13482);
#13502=PRODUCT_DEFINITION('Cage','Cage',#13545,#13482);
#13503=PRODUCT_DEFINITION('Seals 2RS','Seals 2RS',#13546,#13482);
#13504=PRODUCT_DEFINITION('Cap Screw - M5x20','Cap Screw - M5x20',#13547,
#13482);
#13505=PRODUCT_DEFINITION('Linear Ball Bushing - 12 x 21 x 30 mm',
'Linear Ball Bushing - 12 x 21 x 30 mm',#13548,#13482);
#13506=PRODUCT_DEFINITION('Steel sleeve','Steel sleeve',#13549,#13482);
#13507=PRODUCT_DEFINITION('Ball retainer (plastic)',
'Ball retainer (plastic)',#13550,#13482);
#13508=PRODUCT_DEFINITION('M4x10 Cap Screw','M4x10 Cap Screw',#13551,#13482);
#13509=PRODUCT_DEFINITION('Camshaft and hand crank',
'Camshaft and hand crank',#13552,#13482);
#13510=PRODUCT_DEFINITION('Camshaft','Camshaft',#13553,#13482);
#13511=PRODUCT_DEFINITION('Inner race sleeve 10 mm',
'Inner race sleeve 10 mm',#13554,#13482);
#13512=PRODUCT_DEFINITION('Inner race sleeve 10 mm (1)',
'Inner race sleeve 10 mm (1)',#13555,#13482);
#13513=PRODUCT_DEFINITION('Inner race sleeve 15 mm',
'Inner race sleeve 15 mm',#13556,#13482);
#13514=PRODUCT_DEFINITION('Inner race sleeve 15 mm (1)',
'Inner race sleeve 15 mm (1)',#13557,#13482);
#13515=PRODUCT_DEFINITION('Eccentric cam','Eccentric cam',#13558,#13482);
#13516=PRODUCT_DEFINITION('Hand crank','Hand crank',#13559,#13482);
#13517=PRODUCT_DEFINITION('Crank grip','Crank grip',#13560,#13482);
#13518=PRODUCT_DEFINITION('Axial keeper','Axial keeper',#13561,#13482);
#13519=PRODUCT_DEFINITION('Axial keeper (1)','Axial keeper (1)',#13562,#13482);
#13520=PRODUCT_DEFINITION('Key 4x4x14','Key 4x4x14',#13563,#13482);
#13521=PRODUCT_DEFINITION('Cap Screw - M4x16','Cap Screw - M4x16',#13564,
#13482);
#13522=PRODUCT_DEFINITION('Output platform and follower',
'Output platform and follower',#13565,#13482);
#13523=PRODUCT_DEFINITION('Flat follower shoe','Flat follower shoe',#13566,
#13482);
#13524=PRODUCT_DEFINITION('Output stem','Output stem',#13567,#13482);
#13525=PRODUCT_DEFINITION('Spring seat washer','Spring seat washer',#13568,
#13482);
#13526=PRODUCT_DEFINITION_FORMATION('',$,#13615);
#13527=PRODUCT_DEFINITION_FORMATION('',$,#13616);
#13528=PRODUCT_DEFINITION_FORMATION('',$,#13617);
#13529=PRODUCT_DEFINITION_FORMATION('',$,#13618);
#13530=PRODUCT_DEFINITION_FORMATION('',$,#13619);
#13531=PRODUCT_DEFINITION_FORMATION('',$,#13620);
#13532=PRODUCT_DEFINITION_FORMATION('',$,#13621);
#13533=PRODUCT_DEFINITION_FORMATION('',$,#13622);
#13534=PRODUCT_DEFINITION_FORMATION('',$,#13623);
#13535=PRODUCT_DEFINITION_FORMATION('',$,#13624);
#13536=PRODUCT_DEFINITION_FORMATION('',$,#13625);
#13537=PRODUCT_DEFINITION_FORMATION('',$,#13626);
#13538=PRODUCT_DEFINITION_FORMATION('',$,#13627);
#13539=PRODUCT_DEFINITION_FORMATION('',$,#13628);
#13540=PRODUCT_DEFINITION_FORMATION('',$,#13629);
#13541=PRODUCT_DEFINITION_FORMATION('',$,#13630);
#13542=PRODUCT_DEFINITION_FORMATION('',$,#13631);
#13543=PRODUCT_DEFINITION_FORMATION('',$,#13632);
#13544=PRODUCT_DEFINITION_FORMATION('',$,#13633);
#13545=PRODUCT_DEFINITION_FORMATION('',$,#13634);
#13546=PRODUCT_DEFINITION_FORMATION('',$,#13635);
#13547=PRODUCT_DEFINITION_FORMATION('',$,#13636);
#13548=PRODUCT_DEFINITION_FORMATION('',$,#13637);
#13549=PRODUCT_DEFINITION_FORMATION('',$,#13638);
#13550=PRODUCT_DEFINITION_FORMATION('',$,#13639);
#13551=PRODUCT_DEFINITION_FORMATION('',$,#13640);
#13552=PRODUCT_DEFINITION_FORMATION('',$,#13641);
#13553=PRODUCT_DEFINITION_FORMATION('',$,#13642);
#13554=PRODUCT_DEFINITION_FORMATION('',$,#13643);
#13555=PRODUCT_DEFINITION_FORMATION('',$,#13644);
#13556=PRODUCT_DEFINITION_FORMATION('',$,#13645);
#13557=PRODUCT_DEFINITION_FORMATION('',$,#13646);
#13558=PRODUCT_DEFINITION_FORMATION('',$,#13647);
#13559=PRODUCT_DEFINITION_FORMATION('',$,#13648);
#13560=PRODUCT_DEFINITION_FORMATION('',$,#13649);
#13561=PRODUCT_DEFINITION_FORMATION('',$,#13650);
#13562=PRODUCT_DEFINITION_FORMATION('',$,#13651);
#13563=PRODUCT_DEFINITION_FORMATION('',$,#13652);
#13564=PRODUCT_DEFINITION_FORMATION('',$,#13653);
#13565=PRODUCT_DEFINITION_FORMATION('',$,#13654);
#13566=PRODUCT_DEFINITION_FORMATION('',$,#13655);
#13567=PRODUCT_DEFINITION_FORMATION('',$,#13656);
#13568=PRODUCT_DEFINITION_FORMATION('',$,#13657);
#13569=PRODUCT_RELATED_PRODUCT_CATEGORY('PAT-018','PAT-018',(#13615));
#13570=PRODUCT_RELATED_PRODUCT_CATEGORY('Bearing frame and stem guide',
'Bearing frame and stem guide',(#13616));
#13571=PRODUCT_RELATED_PRODUCT_CATEGORY('Base','Base',(#13617));
#13572=PRODUCT_RELATED_PRODUCT_CATEGORY('Foot','Foot',(#13618));
#13573=PRODUCT_RELATED_PRODUCT_CATEGORY('Foot (1)','Foot (1)',(#13619));
#13574=PRODUCT_RELATED_PRODUCT_CATEGORY('Camshaft bearing post',
'Camshaft bearing post',(#13620));
#13575=PRODUCT_RELATED_PRODUCT_CATEGORY('Bearing cap','Bearing cap',(#13621));
#13576=PRODUCT_RELATED_PRODUCT_CATEGORY('Bearing cap (1)',
'Bearing cap (1)',(#13622));
#13577=PRODUCT_RELATED_PRODUCT_CATEGORY('Camshaft bearing post (1)',
'Camshaft bearing post (1)',(#13623));
#13578=PRODUCT_RELATED_PRODUCT_CATEGORY('Bearing cap (2)',
'Bearing cap (2)',(#13624));
#13579=PRODUCT_RELATED_PRODUCT_CATEGORY('Bearing cap (3)',
'Bearing cap (3)',(#13625));
#13580=PRODUCT_RELATED_PRODUCT_CATEGORY('Slide guide bridge',
'Slide guide bridge',(#13626));
#13581=PRODUCT_RELATED_PRODUCT_CATEGORY('Bushing separator',
'Bushing separator',(#13627));
#13582=PRODUCT_RELATED_PRODUCT_CATEGORY('Stem guide cap',
'Stem guide cap',(#13628));
#13583=PRODUCT_RELATED_PRODUCT_CATEGORY('Installed return spring',
'Installed return spring',(#13629));
#13584=PRODUCT_RELATED_PRODUCT_CATEGORY(
'Sealed Ball Bearing - 12 x 32 x 10 mm',
'Sealed Ball Bearing - 12 x 32 x 10 mm',(#13630));
#13585=PRODUCT_RELATED_PRODUCT_CATEGORY('Inner ring','Inner ring',(#13631));
#13586=PRODUCT_RELATED_PRODUCT_CATEGORY('Outer ring','Outer ring',(#13632));
#13587=PRODUCT_RELATED_PRODUCT_CATEGORY('Balls','Balls',(#13633));
#13588=PRODUCT_RELATED_PRODUCT_CATEGORY('Cage','Cage',(#13634));
#13589=PRODUCT_RELATED_PRODUCT_CATEGORY('Seals 2RS','Seals 2RS',(#13635));
#13590=PRODUCT_RELATED_PRODUCT_CATEGORY('Cap Screw - M5x20',
'Cap Screw - M5x20',(#13636));
#13591=PRODUCT_RELATED_PRODUCT_CATEGORY(
'Linear Ball Bushing - 12 x 21 x 30 mm',
'Linear Ball Bushing - 12 x 21 x 30 mm',(#13637));
#13592=PRODUCT_RELATED_PRODUCT_CATEGORY('Steel sleeve','Steel sleeve',(#13638));
#13593=PRODUCT_RELATED_PRODUCT_CATEGORY('Ball retainer (plastic)',
'Ball retainer (plastic)',(#13639));
#13594=PRODUCT_RELATED_PRODUCT_CATEGORY('M4x10 Cap Screw',
'M4x10 Cap Screw',(#13640));
#13595=PRODUCT_RELATED_PRODUCT_CATEGORY('Camshaft and hand crank',
'Camshaft and hand crank',(#13641));
#13596=PRODUCT_RELATED_PRODUCT_CATEGORY('Camshaft','Camshaft',(#13642));
#13597=PRODUCT_RELATED_PRODUCT_CATEGORY('Inner race sleeve 10 mm',
'Inner race sleeve 10 mm',(#13643));
#13598=PRODUCT_RELATED_PRODUCT_CATEGORY('Inner race sleeve 10 mm (1)',
'Inner race sleeve 10 mm (1)',(#13644));
#13599=PRODUCT_RELATED_PRODUCT_CATEGORY('Inner race sleeve 15 mm',
'Inner race sleeve 15 mm',(#13645));
#13600=PRODUCT_RELATED_PRODUCT_CATEGORY('Inner race sleeve 15 mm (1)',
'Inner race sleeve 15 mm (1)',(#13646));
#13601=PRODUCT_RELATED_PRODUCT_CATEGORY('Eccentric cam','Eccentric cam',
(#13647));
#13602=PRODUCT_RELATED_PRODUCT_CATEGORY('Hand crank','Hand crank',(#13648));
#13603=PRODUCT_RELATED_PRODUCT_CATEGORY('Crank grip','Crank grip',(#13649));
#13604=PRODUCT_RELATED_PRODUCT_CATEGORY('Axial keeper','Axial keeper',(#13650));
#13605=PRODUCT_RELATED_PRODUCT_CATEGORY('Axial keeper (1)',
'Axial keeper (1)',(#13651));
#13606=PRODUCT_RELATED_PRODUCT_CATEGORY('Key 4x4x14','Key 4x4x14',(#13652));
#13607=PRODUCT_RELATED_PRODUCT_CATEGORY('Cap Screw - M4x16',
'Cap Screw - M4x16',(#13653));
#13608=PRODUCT_RELATED_PRODUCT_CATEGORY('Output platform and follower',
'Output platform and follower',(#13654));
#13609=PRODUCT_RELATED_PRODUCT_CATEGORY('Flat follower shoe',
'Flat follower shoe',(#13655));
#13610=PRODUCT_RELATED_PRODUCT_CATEGORY('Output stem','Output stem',(#13656));
#13611=PRODUCT_RELATED_PRODUCT_CATEGORY('Spring seat washer',
'Spring seat washer',(#13657));
#13612=APPLICATION_PROTOCOL_DEFINITION('international standard',
'automotive_design',2009,#13613);
#13613=APPLICATION_CONTEXT(
'Core Data for Automotive Mechanical Design Process');
#13614=PRODUCT_CONTEXT('part definition',#13613,'mechanical');
#13615=PRODUCT('PAT-018','PAT-018',
'PAT-018',(#13614));
#13616=PRODUCT('Bearing frame and stem guide',
'Bearing frame and stem guide','Bearing frame and stem guide',(#13614));
#13617=PRODUCT('Base','Base','Base',(#13614));
#13618=PRODUCT('Foot','Foot','Foot',(#13614));
#13619=PRODUCT('Foot (1)','Foot (1)','Foot (1)',(#13614));
#13620=PRODUCT('Camshaft bearing post','Camshaft bearing post',
'Camshaft bearing post',(#13614));
#13621=PRODUCT('Bearing cap','Bearing cap','Bearing cap',(#13614));
#13622=PRODUCT('Bearing cap (1)','Bearing cap (1)','Bearing cap (1)',(#13614));
#13623=PRODUCT('Camshaft bearing post (1)','Camshaft bearing post (1)',
'Camshaft bearing post (1)',(#13614));
#13624=PRODUCT('Bearing cap (2)','Bearing cap (2)','Bearing cap (2)',(#13614));
#13625=PRODUCT('Bearing cap (3)','Bearing cap (3)','Bearing cap (3)',(#13614));
#13626=PRODUCT('Slide guide bridge','Slide guide bridge',
'Slide guide bridge',(#13614));
#13627=PRODUCT('Bushing separator','Bushing separator',
'Bushing separator',(#13614));
#13628=PRODUCT('Stem guide cap','Stem guide cap','Stem guide cap',(#13614));
#13629=PRODUCT('Installed return spring','Installed return spring',
'Installed return spring',(#13614));
#13630=PRODUCT('Sealed Ball Bearing - 12 x 32 x 10 mm',
'Sealed Ball Bearing - 12 x 32 x 10 mm',
'Sealed Ball Bearing - 12 x 32 x 10 mm',(#13614));
#13631=PRODUCT('Inner ring','Inner ring','Inner ring',(#13614));
#13632=PRODUCT('Outer ring','Outer ring','Outer ring',(#13614));
#13633=PRODUCT('Balls','Balls','Balls',(#13614));
#13634=PRODUCT('Cage','Cage','Cage',(#13614));
#13635=PRODUCT('Seals 2RS','Seals 2RS','Seals 2RS',(#13614));
#13636=PRODUCT('Cap Screw - M5x20','Cap Screw - M5x20',
'Cap Screw - M5x20',(#13614));
#13637=PRODUCT('Linear Ball Bushing - 12 x 21 x 30 mm',
'Linear Ball Bushing - 12 x 21 x 30 mm',
'Linear Ball Bushing - 12 x 21 x 30 mm',(#13614));
#13638=PRODUCT('Steel sleeve','Steel sleeve','Steel sleeve',(#13614));
#13639=PRODUCT('Ball retainer (plastic)','Ball retainer (plastic)',
'Ball retainer (plastic)',(#13614));
#13640=PRODUCT('M4x10 Cap Screw','M4x10 Cap Screw','M4x10 Cap Screw',(#13614));
#13641=PRODUCT('Camshaft and hand crank','Camshaft and hand crank',
'Camshaft and hand crank',(#13614));
#13642=PRODUCT('Camshaft','Camshaft','Camshaft',(#13614));
#13643=PRODUCT('Inner race sleeve 10 mm','Inner race sleeve 10 mm',
'Inner race sleeve 10 mm',(#13614));
#13644=PRODUCT('Inner race sleeve 10 mm (1)',
'Inner race sleeve 10 mm (1)','Inner race sleeve 10 mm (1)',(#13614));
#13645=PRODUCT('Inner race sleeve 15 mm','Inner race sleeve 15 mm',
'Inner race sleeve 15 mm',(#13614));
#13646=PRODUCT('Inner race sleeve 15 mm (1)',
'Inner race sleeve 15 mm (1)','Inner race sleeve 15 mm (1)',(#13614));
#13647=PRODUCT('Eccentric cam','Eccentric cam','Eccentric cam',(#13614));
#13648=PRODUCT('Hand crank','Hand crank','Hand crank',(#13614));
#13649=PRODUCT('Crank grip','Crank grip','Crank grip',(#13614));
#13650=PRODUCT('Axial keeper','Axial keeper','Axial keeper',(#13614));
#13651=PRODUCT('Axial keeper (1)','Axial keeper (1)','Axial keeper (1)',(#13614));
#13652=PRODUCT('Key 4x4x14','Key 4x4x14','Key 4x4x14',(#13614));
#13653=PRODUCT('Cap Screw - M4x16','Cap Screw - M4x16',
'Cap Screw - M4x16',(#13614));
#13654=PRODUCT('Output platform and follower',
'Output platform and follower','Output platform and follower',(#13614));
#13655=PRODUCT('Flat follower shoe','Flat follower shoe',
'Flat follower shoe',(#13614));
#13656=PRODUCT('Output stem','Output stem','Output stem',(#13614));
#13657=PRODUCT('Spring seat washer','Spring seat washer',
'Spring seat washer',(#13614));
#13658=PRESENTATION_STYLE_ASSIGNMENT((#13663));
#13659=PRESENTATION_STYLE_ASSIGNMENT((#13664));
#13660=PRESENTATION_STYLE_ASSIGNMENT((#13665));
#13661=PRESENTATION_STYLE_ASSIGNMENT((#13666));
#13662=PRESENTATION_STYLE_ASSIGNMENT((#13667));
#13663=SURFACE_STYLE_USAGE(.BOTH.,#13668);
#13664=SURFACE_STYLE_USAGE(.BOTH.,#13669);
#13665=SURFACE_STYLE_USAGE(.BOTH.,#13670);
#13666=SURFACE_STYLE_USAGE(.BOTH.,#13671);
#13667=SURFACE_STYLE_USAGE(.BOTH.,#13672);
#13668=SURFACE_SIDE_STYLE('',(#13673));
#13669=SURFACE_SIDE_STYLE('',(#13674));
#13670=SURFACE_SIDE_STYLE('',(#13675));
#13671=SURFACE_SIDE_STYLE('',(#13676));
#13672=SURFACE_SIDE_STYLE('',(#13677));
#13673=SURFACE_STYLE_FILL_AREA(#13678);
#13674=SURFACE_STYLE_FILL_AREA(#13679);
#13675=SURFACE_STYLE_FILL_AREA(#13680);
#13676=SURFACE_STYLE_FILL_AREA(#13681);
#13677=SURFACE_STYLE_FILL_AREA(#13682);
#13678=FILL_AREA_STYLE('Steel - Satin',(#13683));
#13679=FILL_AREA_STYLE('CAD Library Painted - Deep blue',(#13684));
#13680=FILL_AREA_STYLE('CAD Library Painted - Steel gray',(#13685));
#13681=FILL_AREA_STYLE('CAD Library Painted - Engineering blue',(#13686));
#13682=FILL_AREA_STYLE('CAD Library Painted - Graphite',(#13687));
#13683=FILL_AREA_STYLE_COLOUR('Steel - Satin',#13688);
#13684=FILL_AREA_STYLE_COLOUR('CAD Library Painted - Deep blue',#13689);
#13685=FILL_AREA_STYLE_COLOUR('CAD Library Painted - Steel gray',#13690);
#13686=FILL_AREA_STYLE_COLOUR('CAD Library Painted - Engineering blue',
#13691);
#13687=FILL_AREA_STYLE_COLOUR('CAD Library Painted - Graphite',#13692);
#13688=COLOUR_RGB('Steel - Satin',0.627450980392157,0.627450980392157,0.627450980392157);
#13689=COLOUR_RGB('CAD Library Painted - Deep blue',0.0784313725490196,
0.203921568627451,0.349019607843137);
#13690=COLOUR_RGB('CAD Library Painted - Steel gray',0.592156862745098,
0.631372549019608,0.67843137254902);
#13691=COLOUR_RGB('CAD Library Painted - Engineering blue',0.12156862745098,
0.356862745098039,0.6);
#13692=COLOUR_RGB('CAD Library Painted - Graphite',0.168627450980392,0.192156862745098,
0.231372549019608);
#13693=COLOUR_RGB('Dark Blue',0.08,0.2,0.34);
#13694=FILL_AREA_STYLE_COLOUR('',#13693);
#13695=FILL_AREA_STYLE('',(#13694));
#13696=SURFACE_STYLE_FILL_AREA(#13695);
#13697=SURFACE_SIDE_STYLE('',(#13696));
#13698=SURFACE_STYLE_USAGE(.BOTH.,#13697);
#13699=PRESENTATION_STYLE_ASSIGNMENT((#13698));
#13700=COLOUR_RGB('Light Blue',0.38,0.62,0.78);
#13701=FILL_AREA_STYLE_COLOUR('',#13700);
#13702=FILL_AREA_STYLE('',(#13701));
#13703=SURFACE_STYLE_FILL_AREA(#13702);
#13704=SURFACE_SIDE_STYLE('',(#13703));
#13705=SURFACE_STYLE_USAGE(.BOTH.,#13704);
#13706=PRESENTATION_STYLE_ASSIGNMENT((#13705));
#13707=COLOUR_RGB('Sky Blue',0.24,0.69,0.87);
#13708=FILL_AREA_STYLE_COLOUR('',#13707);
#13709=FILL_AREA_STYLE('',(#13708));
#13710=SURFACE_STYLE_FILL_AREA(#13709);
#13711=SURFACE_SIDE_STYLE('',(#13710));
#13712=SURFACE_STYLE_USAGE(.BOTH.,#13711);
#13713=PRESENTATION_STYLE_ASSIGNMENT((#13712));
#13714=COLOUR_RGB('Grey',0.48,0.52,0.57);
#13715=FILL_AREA_STYLE_COLOUR('',#13714);
#13716=FILL_AREA_STYLE('',(#13715));
#13717=SURFACE_STYLE_FILL_AREA(#13716);
#13718=SURFACE_SIDE_STYLE('',(#13717));
#13719=SURFACE_STYLE_USAGE(.BOTH.,#13718);
#13720=PRESENTATION_STYLE_ASSIGNMENT((#13719));
#13721=COLOUR_RGB('Black',0.12,0.14,0.17);
#13722=FILL_AREA_STYLE_COLOUR('',#13721);
#13723=FILL_AREA_STYLE('',(#13722));
#13724=SURFACE_STYLE_FILL_AREA(#13723);
#13725=SURFACE_SIDE_STYLE('',(#13724));
#13726=SURFACE_STYLE_USAGE(.BOTH.,#13725);
#13727=PRESENTATION_STYLE_ASSIGNMENT((#13726));
#13728=COLOUR_RGB('Off White',0.89,0.88,0.83);
#13729=FILL_AREA_STYLE_COLOUR('',#13728);
#13730=FILL_AREA_STYLE('',(#13729));
#13731=SURFACE_STYLE_FILL_AREA(#13730);
#13732=SURFACE_SIDE_STYLE('',(#13731));
#13733=SURFACE_STYLE_USAGE(.BOTH.,#13732);
#13734=PRESENTATION_STYLE_ASSIGNMENT((#13733));
ENDSEC;
END-ISO-10303-21;
